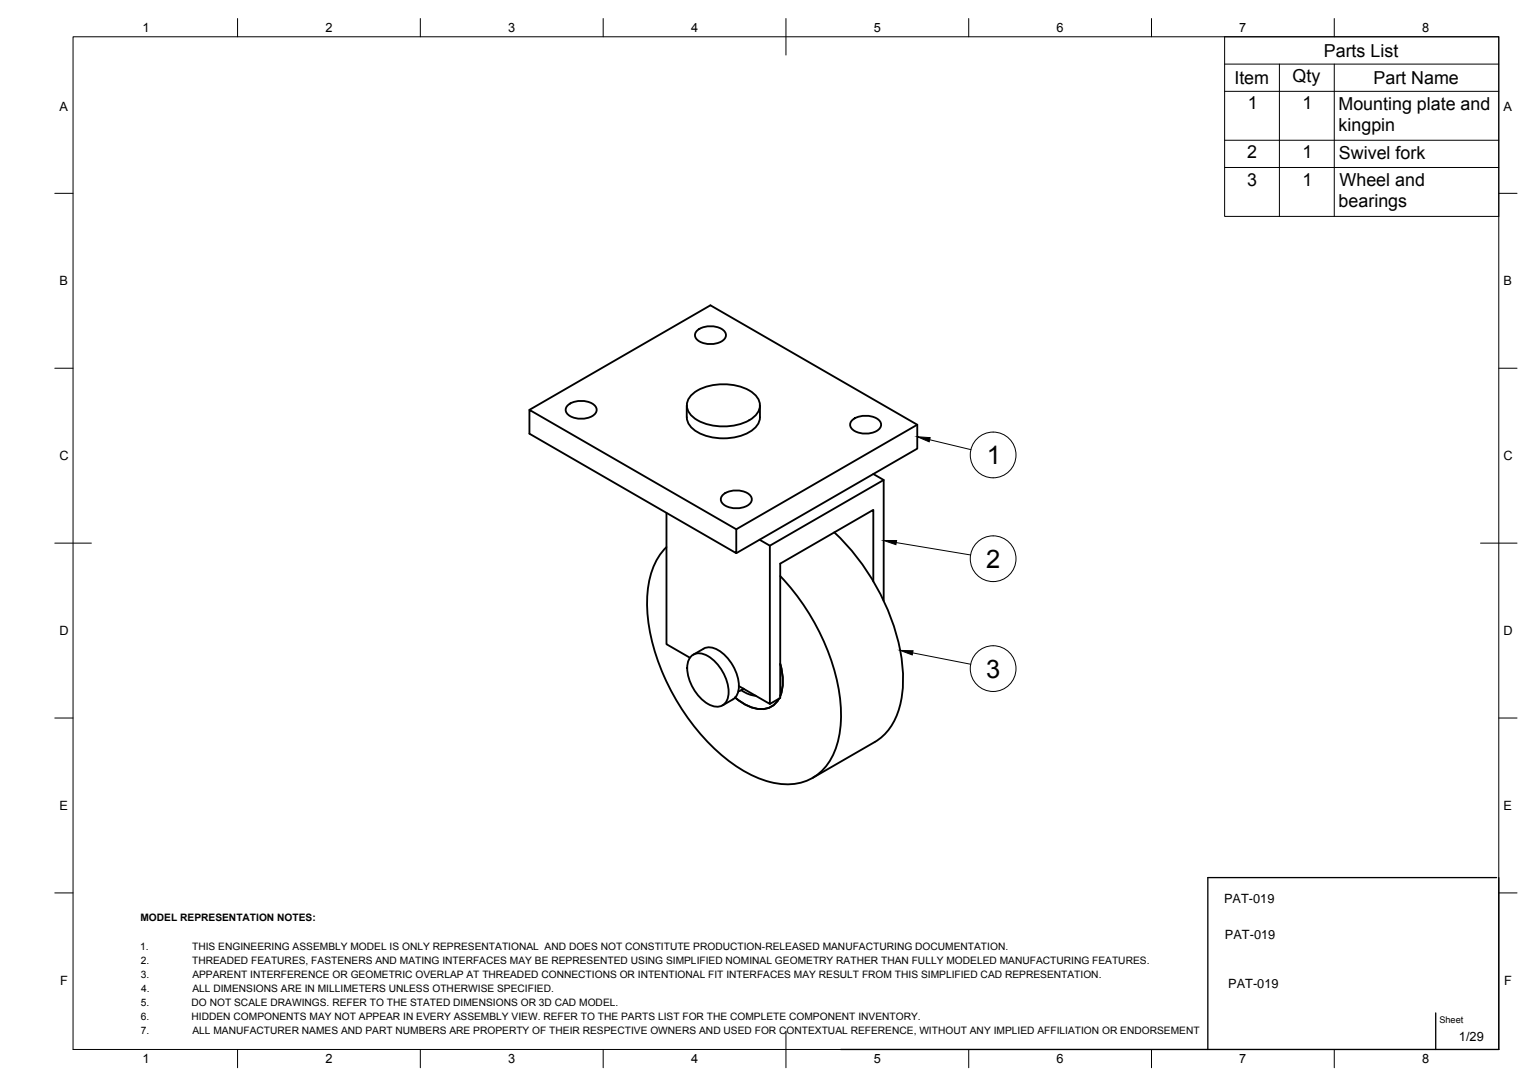
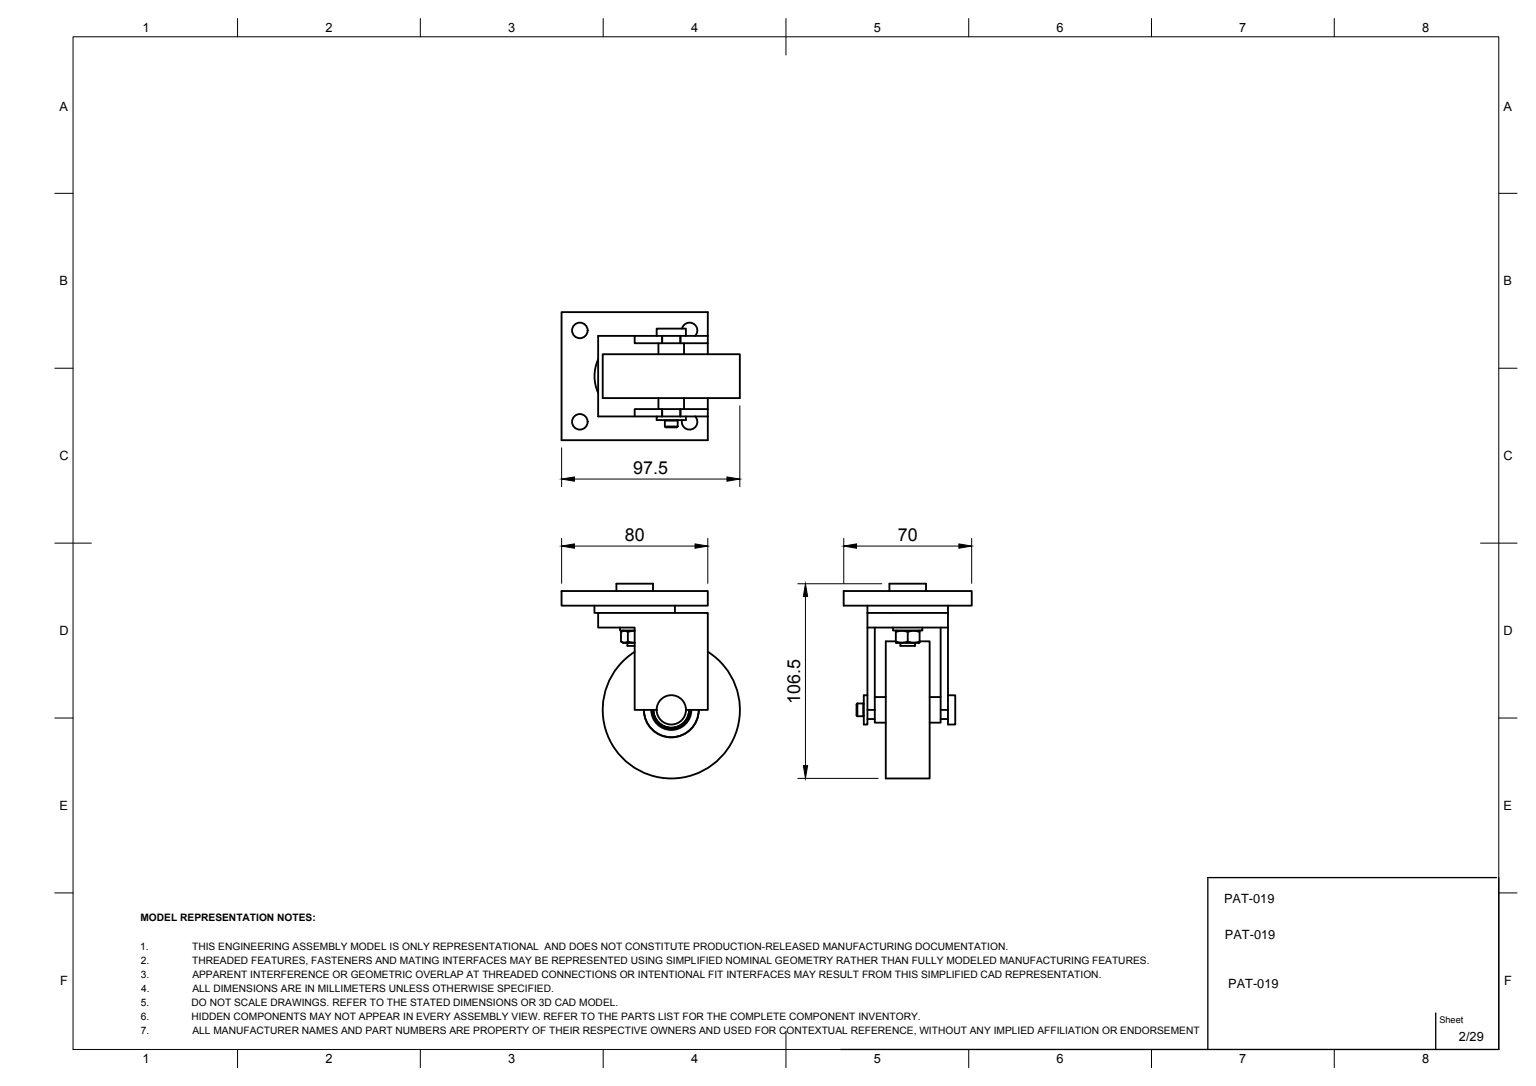
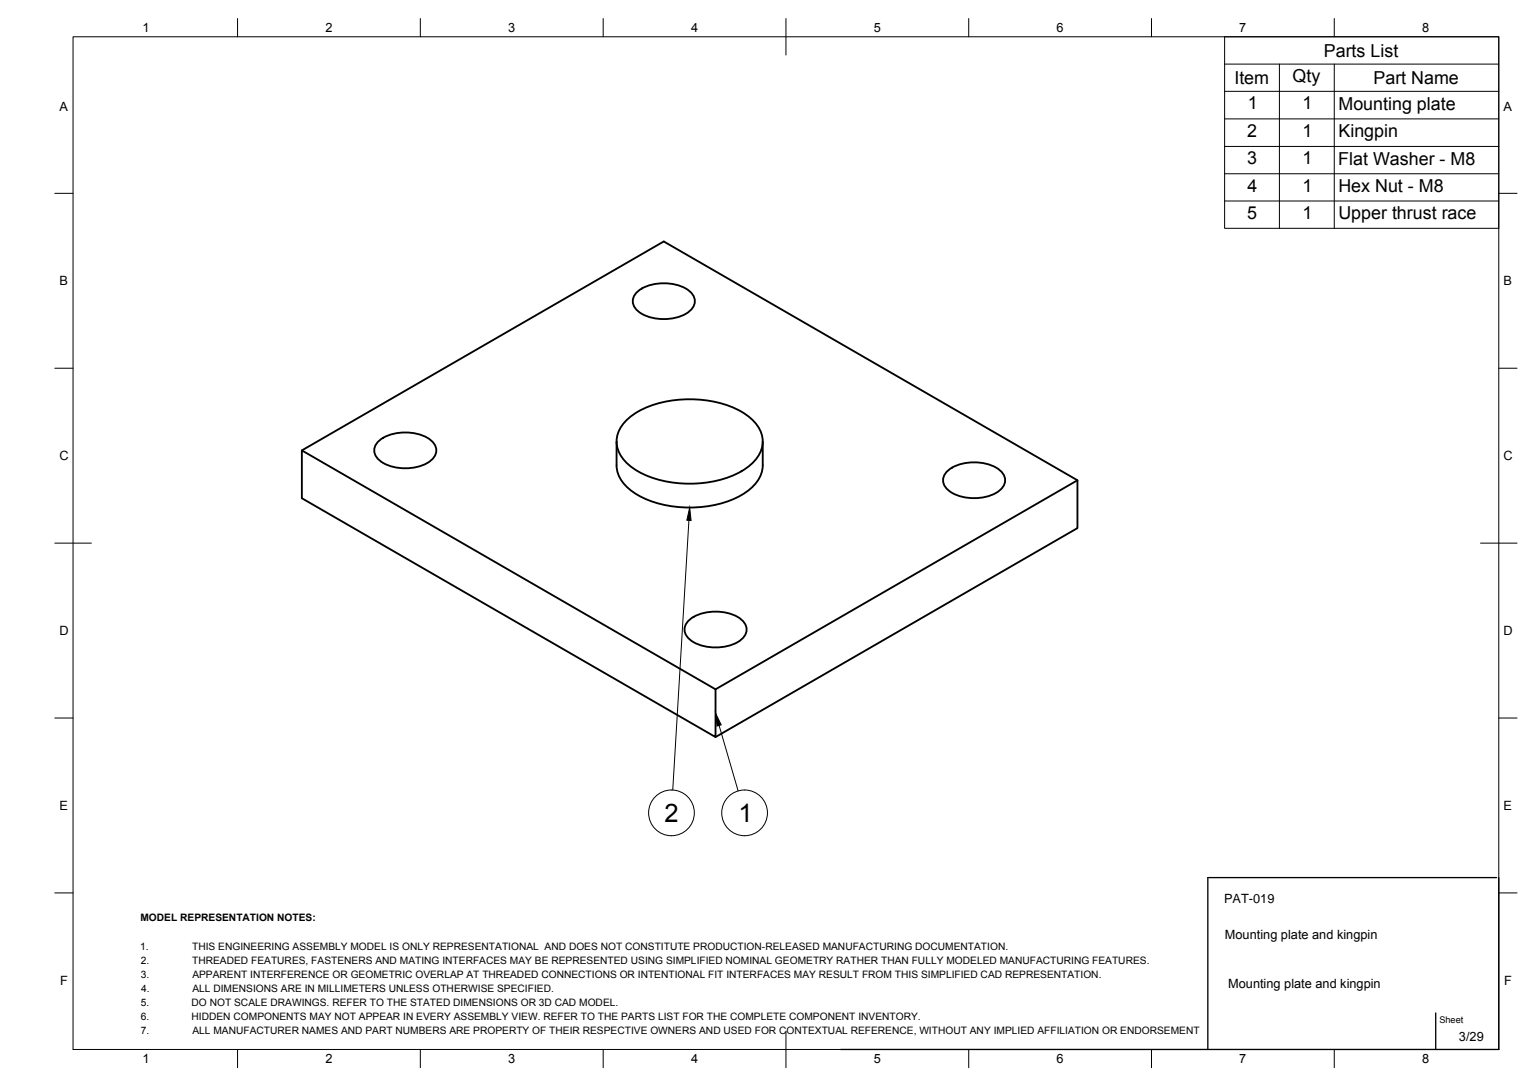
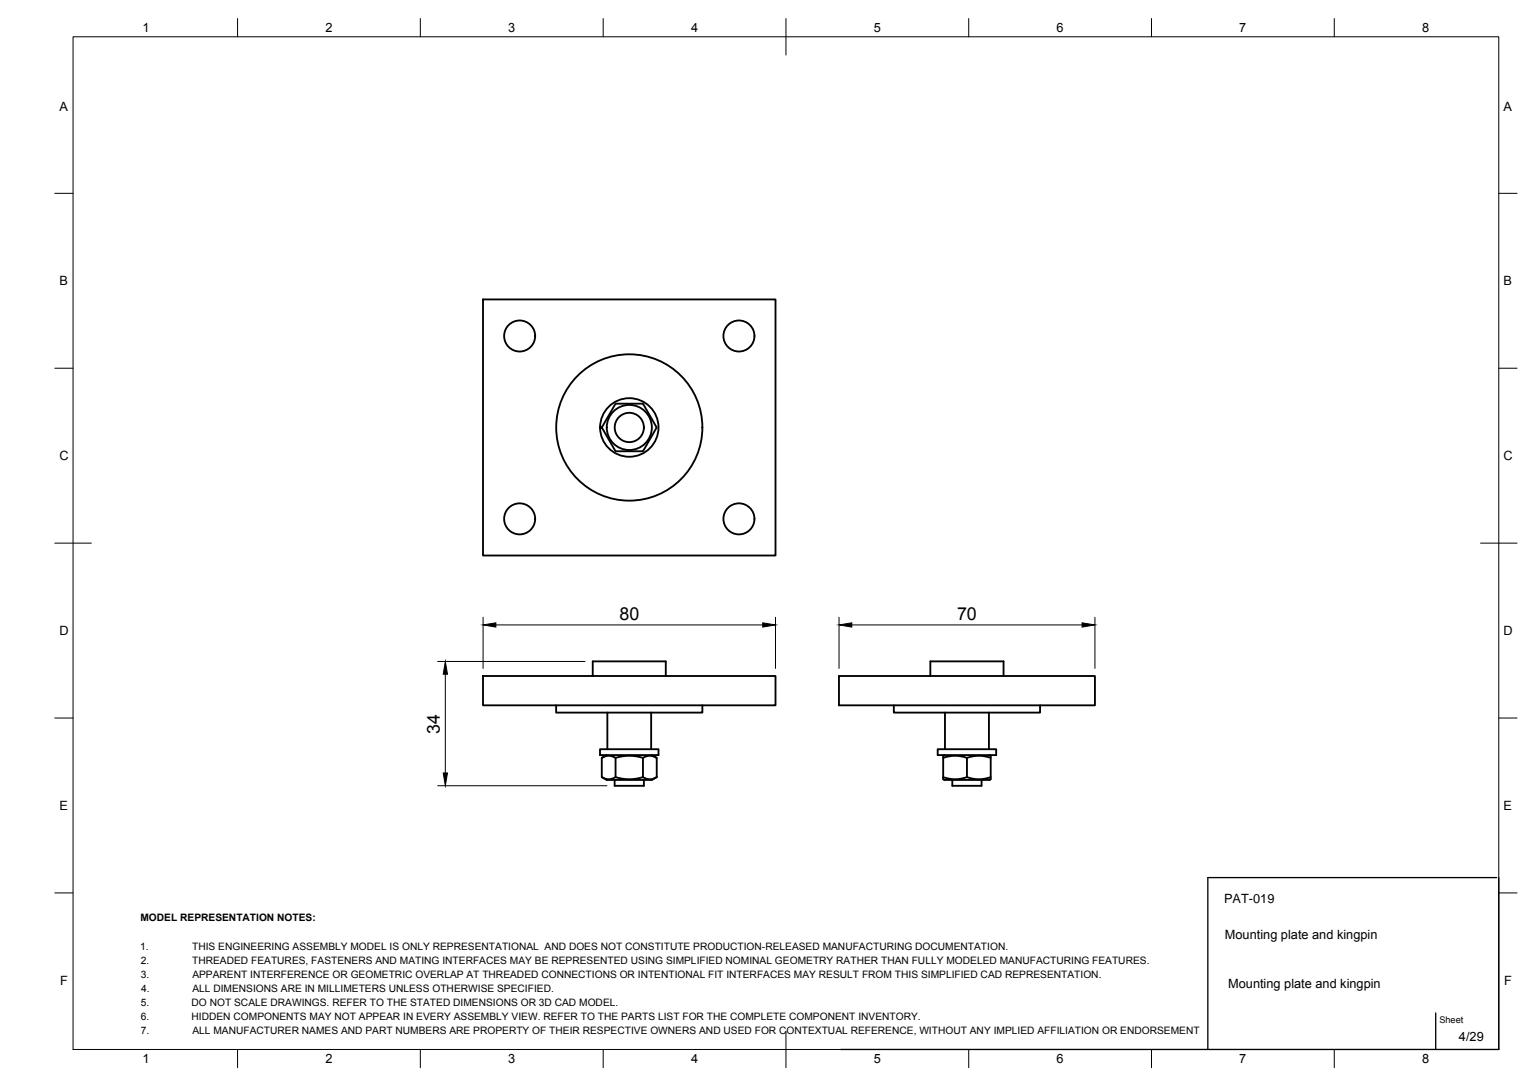
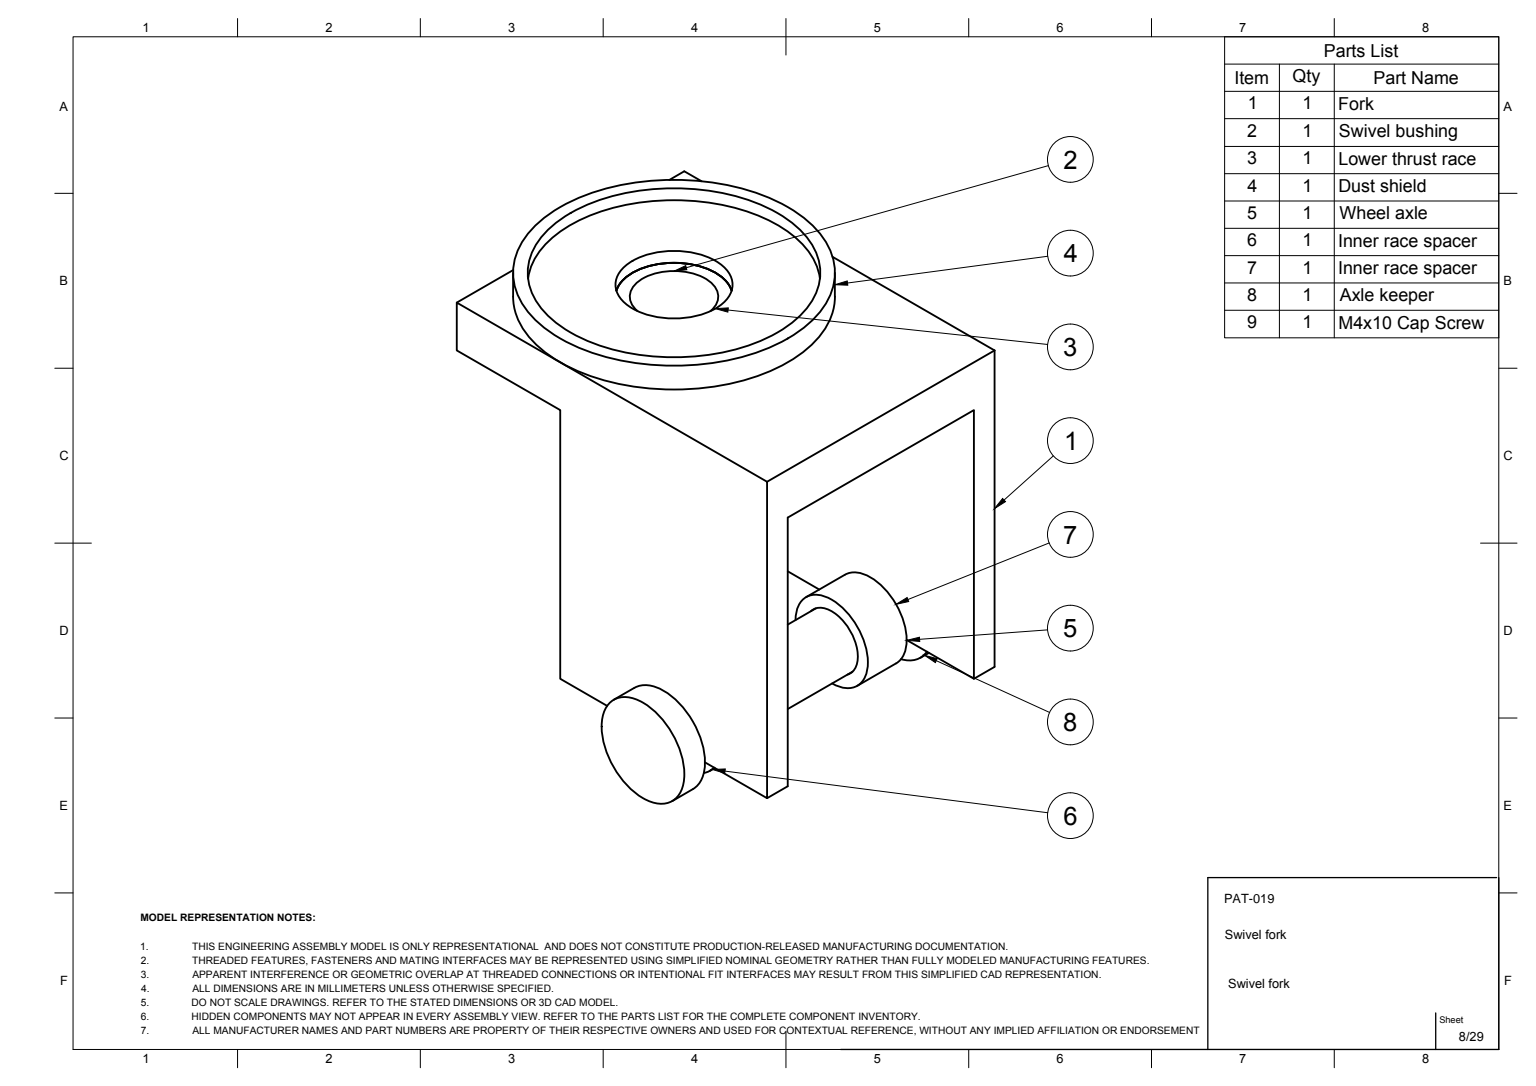
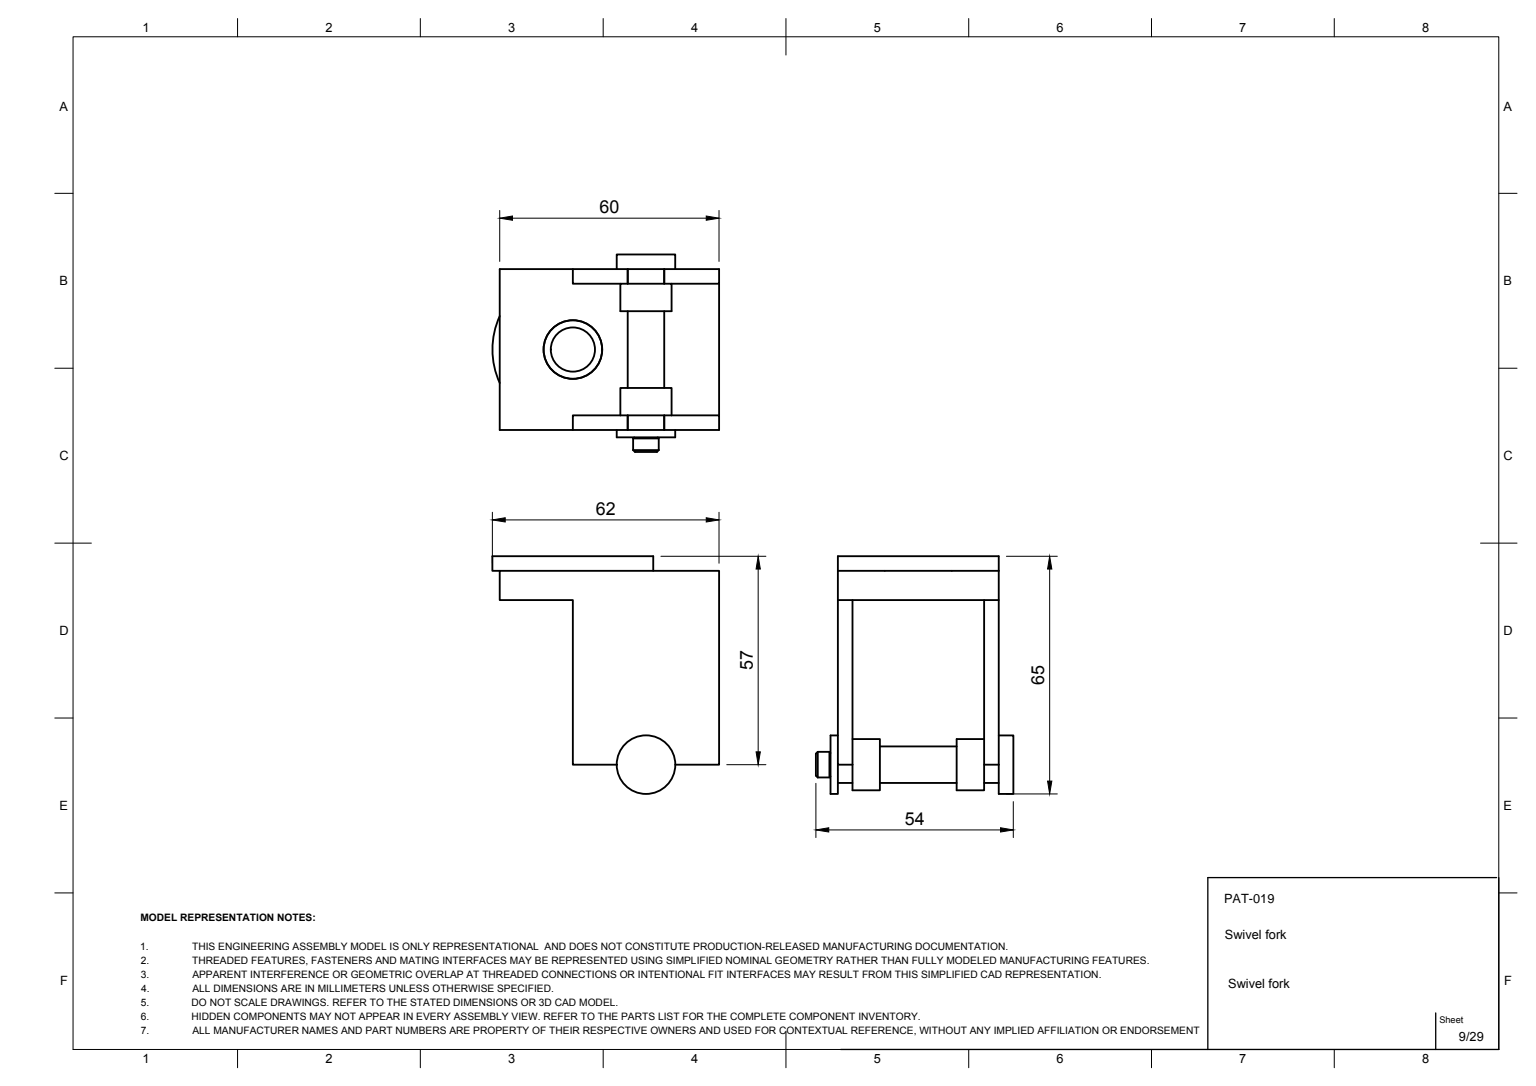
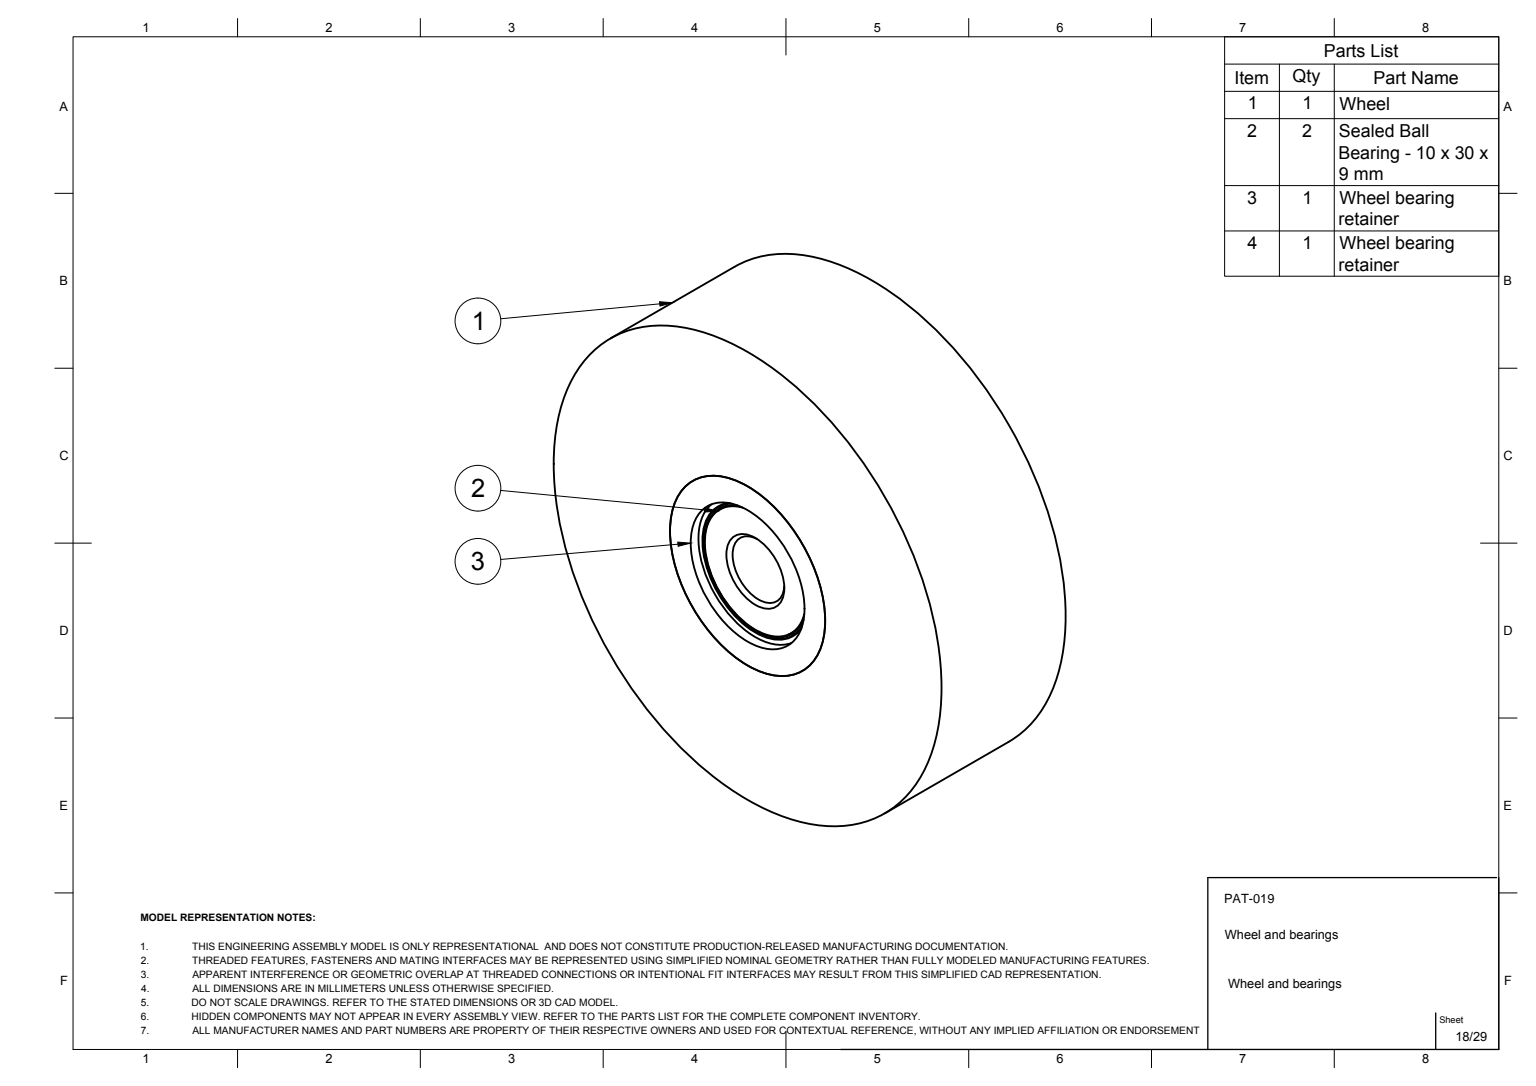
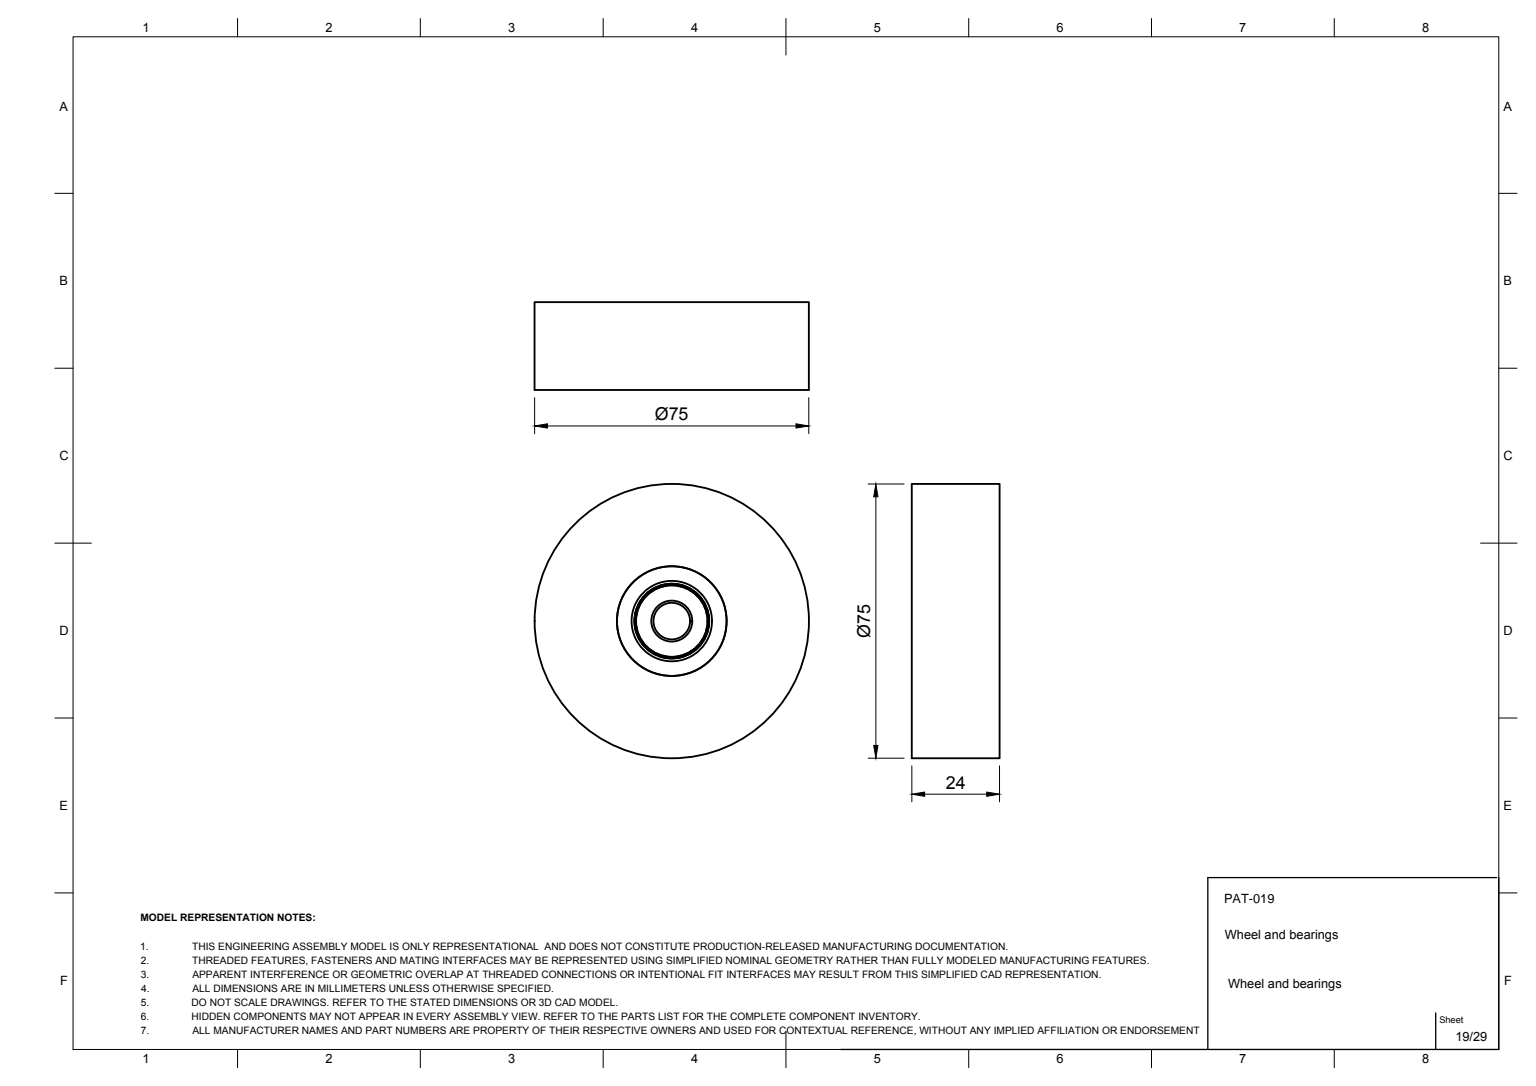
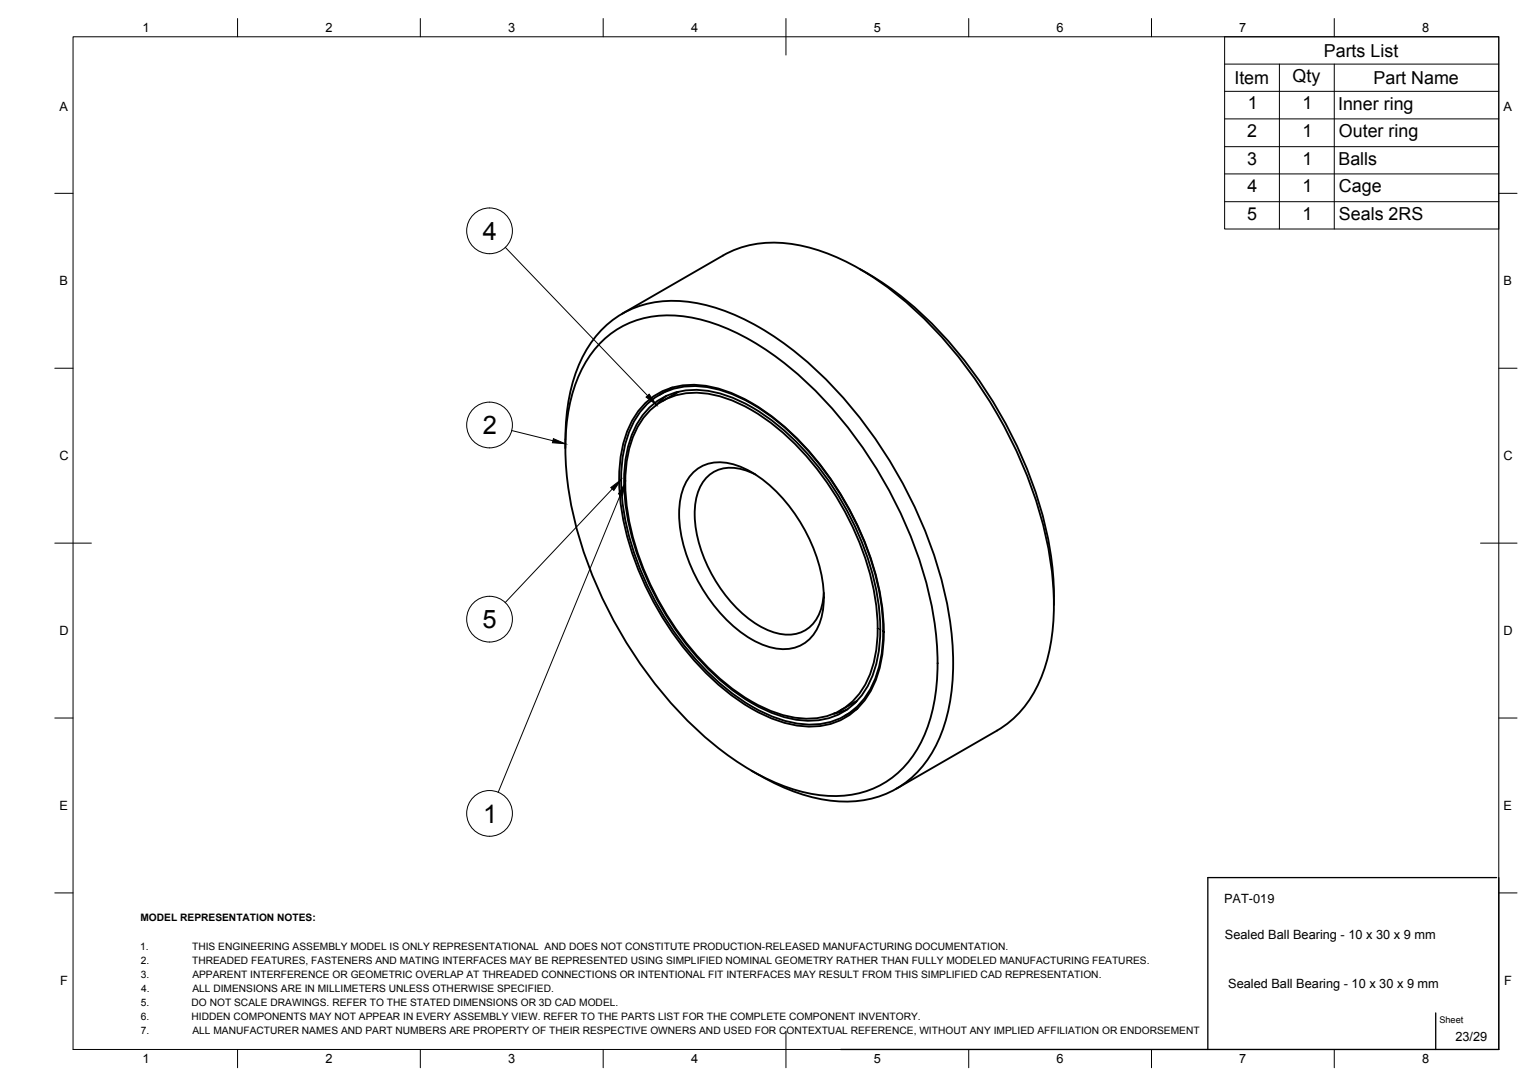
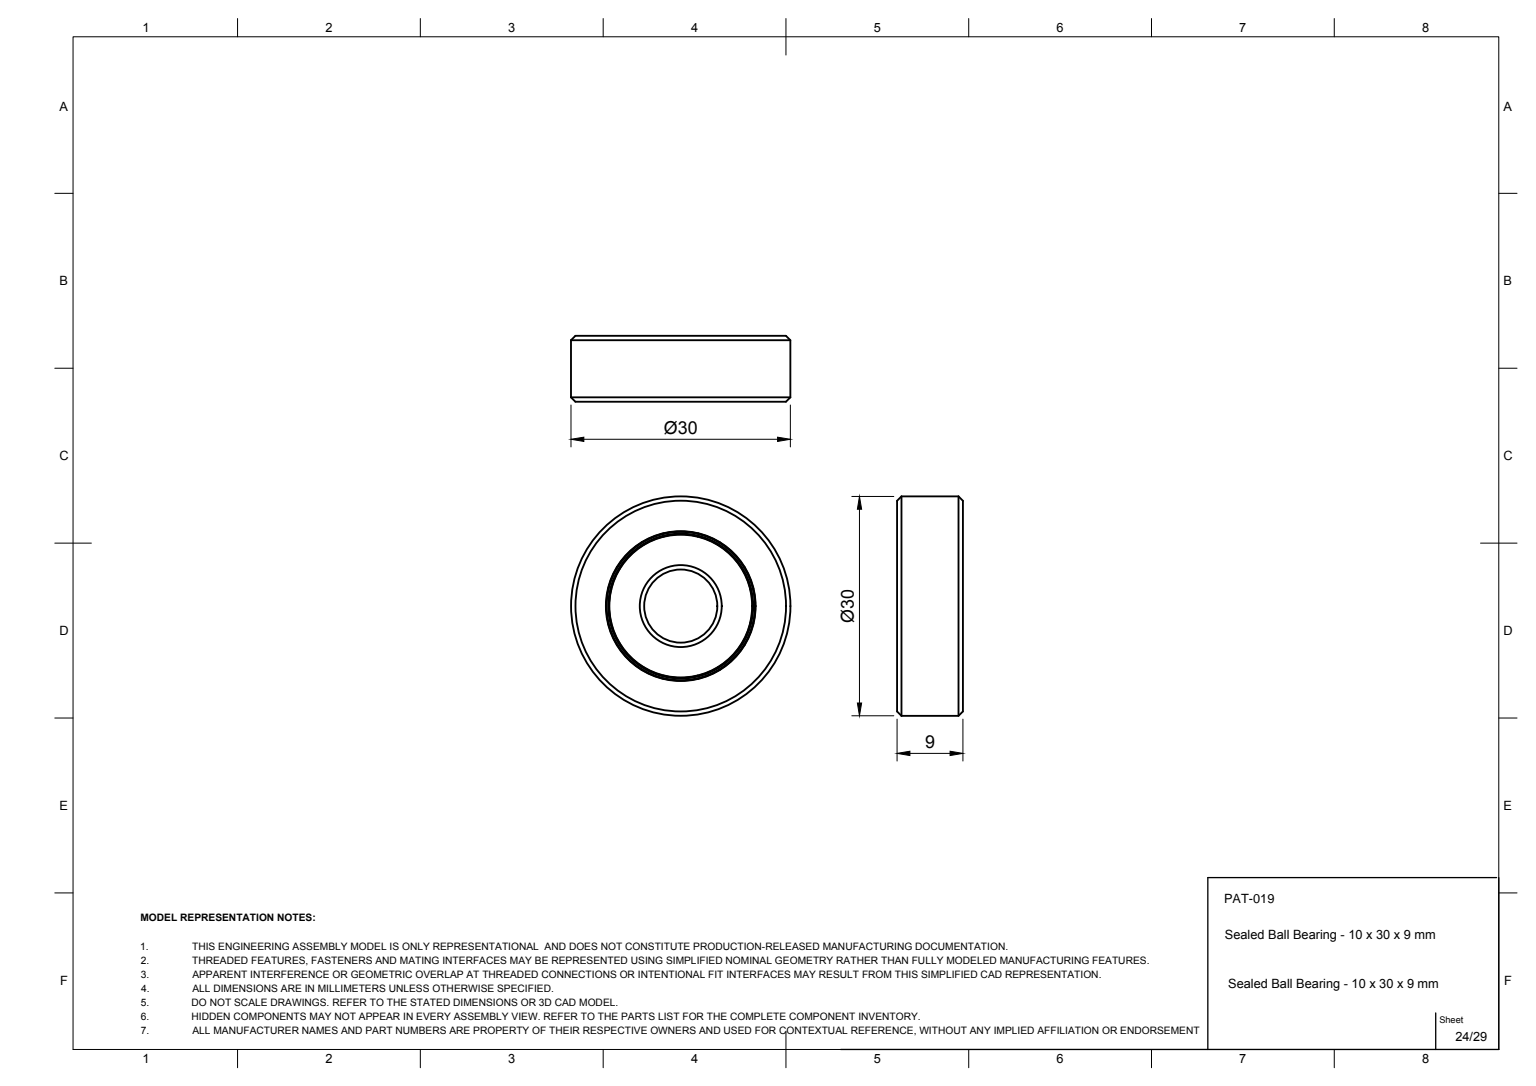
ISO-10303-21;
HEADER;
/* Generated by software containing ST-Developer
 * from STEP Tools, Inc. (www.steptools.com) 
 */

FILE_DESCRIPTION(
/* description */ ('Caster wheel assembly'),
/* implementation_level */ '2;1');

FILE_NAME(
/* name */ 'PAT-019',
/* time_stamp */ '2026-10-28T03:23:56-07:00',
/* author */ (''),
/* organization */ (''),
/* preprocessor_version */ 'ST-DEVELOPER v20.2',
/* originating_system */ 'Autodesk Translation Framework v15.17.0.0',
/* authorisation */ '');

FILE_SCHEMA (('AUTOMOTIVE_DESIGN { 1 0 10303 214 3 1 1 }'));
ENDSEC;

DATA;
#10=MECHANICAL_DESIGN_GEOMETRIC_PRESENTATION_REPRESENTATION('',(#222,#223,
#224,#225,#226,#227,#228,#229,#230,#231,#232,#233,#234,#235,#236,#237,#238,
#239,#240,#241,#242,#243,#244,#245,#246,#247,#248,#249,#250,#251),#5385);
#11=B_SPLINE_CURVE_WITH_KNOTS('',3,(#4844,#4845,#4846,#4847,#4848,#4849,
#4850,#4851,#4852,#4853,#4854,#4855,#4856,#4857,#4858,#4859,#4860,#4861,
#4862,#4863,#4864,#4865),.UNSPECIFIED.,.F.,.F.,(4,2,2,2,2,2,2,2,2,2,4),
(0.0473477652366656,0.126350602536658,0.189525903804987,0.252701205073317,
0.313298422430275,0.373895639787233,0.434492857144191,0.495090074501149,
0.558265375769478,0.621440677037807,0.7004435143378),.UNSPECIFIED.);
#12=B_SPLINE_CURVE_WITH_KNOTS('',3,(#4869,#4870,#4871,#4872,#4873,#4874,
#4875,#4876,#4877,#4878,#4879,#4880,#4881,#4882,#4883,#4884,#4885,#4886,
#4887,#4888,#4889,#4890),.UNSPECIFIED.,.F.,.F.,(4,2,2,2,2,2,2,2,2,2,4),
(0.0464897534940957,0.0852567806515119,0.170513561303024,0.246687263103517,
0.308657850341199,0.370628437578881,0.432599024816563,0.494569612054245,
0.570743313854739,0.656000094506251,0.694767121663666),.UNSPECIFIED.);
#13=B_SPLINE_CURVE_WITH_KNOTS('',3,(#4896,#4897,#4898,#4899,#4900,#4901,
#4902,#4903,#4904,#4905,#4906,#4907,#4908,#4909,#4910,#4911,#4912,#4913,
#4914,#4915,#4916,#4917),.UNSPECIFIED.,.F.,.F.,(4,2,2,2,2,2,2,2,2,2,4),
(0.0464897534940957,0.0852567806515118,0.170513561303024,0.246687263103517,
0.308657850341199,0.370628437578881,0.432599024816563,0.494569612054245,
0.570743313854738,0.65600009450625,0.694767121663666),.UNSPECIFIED.);
#14=B_SPLINE_CURVE_WITH_KNOTS('',3,(#4921,#4922,#4923,#4924,#4925,#4926,
#4927,#4928,#4929,#4930,#4931,#4932,#4933,#4934,#4935,#4936,#4937,#4938,
#4939,#4940,#4941,#4942),.UNSPECIFIED.,.F.,.F.,(4,2,2,2,2,2,2,2,2,2,4),
(0.0464897534940957,0.0852567806515119,0.170513561303024,0.246687263103517,
0.308657850341199,0.370628437578881,0.432599024816563,0.494569612054245,
0.570743313854739,0.656000094506251,0.694767121663666),.UNSPECIFIED.);
#15=B_SPLINE_CURVE_WITH_KNOTS('',3,(#4946,#4947,#4948,#4949,#4950,#4951,
#4952,#4953,#4954,#4955,#4956,#4957),.UNSPECIFIED.,.F.,.F.,(4,2,2,2,2,4),
(0.0464897534940957,0.0852567806515119,0.170513561303024,0.246687263103517,
0.308657850341199,0.370628437578881),.UNSPECIFIED.);
#16=B_SPLINE_CURVE_WITH_KNOTS('',3,(#4962,#4963,#4964,#4965,#4966,#4967,
#4968,#4969,#4970,#4971,#4972,#4973),.UNSPECIFIED.,.F.,.F.,(4,2,2,2,2,4),
(0.370628437578881,0.432599024816563,0.494569612054245,0.570743313854738,
0.65600009450625,0.694767121663666),.UNSPECIFIED.);
#17=B_SPLINE_CURVE_WITH_KNOTS('',3,(#4977,#4978,#4979,#4980,#4981,#4982,
#4983,#4984,#4985,#4986,#4987,#4988,#4989,#4990,#4991,#4992,#4993,#4994,
#4995,#4996,#4997,#4998),.UNSPECIFIED.,.F.,.F.,(4,2,2,2,2,2,2,2,2,2,4),
(0.0464897534940957,0.0852567806515121,0.170513561303024,0.246687263103518,
0.308657850341199,0.370628437578881,0.432599024816563,0.494569612054245,
0.570743313854738,0.65600009450625,0.694767121663666),.UNSPECIFIED.);
#18=B_SPLINE_CURVE_WITH_KNOTS('',3,(#5002,#5003,#5004,#5005,#5006,#5007,
#5008,#5009,#5010,#5011,#5012,#5013,#5014,#5015,#5016,#5017,#5018,#5019,
#5020,#5021,#5022,#5023),.UNSPECIFIED.,.F.,.F.,(4,2,2,2,2,2,2,2,2,2,4),
(0.0464897534940957,0.0852567806515119,0.170513561303024,0.246687263103517,
0.308657850341199,0.370628437578881,0.432599024816563,0.494569612054245,
0.570743313854738,0.65600009450625,0.694767121663667),.UNSPECIFIED.);
#19=B_SPLINE_CURVE_WITH_KNOTS('',3,(#5027,#5028,#5029,#5030,#5031,#5032,
#5033,#5034,#5035,#5036,#5037,#5038,#5039,#5040,#5041,#5042,#5043,#5044,
#5045,#5046,#5047,#5048),.UNSPECIFIED.,.F.,.F.,(4,2,2,2,2,2,2,2,2,2,4),
(0.0464897534940957,0.0852567806515119,0.170513561303024,0.246687263103517,
0.308657850341199,0.370628437578881,0.432599024816563,0.494569612054245,
0.570743313854738,0.65600009450625,0.694767121663666),.UNSPECIFIED.);
#20=B_SPLINE_CURVE_WITH_KNOTS('',3,(#5052,#5053,#5054,#5055,#5056,#5057,
#5058,#5059,#5060,#5061,#5062,#5063,#5064,#5065,#5066,#5067,#5068,#5069,
#5070,#5071,#5072,#5073),.UNSPECIFIED.,.F.,.F.,(4,2,2,2,2,2,2,2,2,2,4),
(0.0464897534940957,0.0852567806515119,0.170513561303024,0.246687263103517,
0.308657850341199,0.370628437578881,0.432599024816563,0.494569612054245,
0.570743313854739,0.656000094506251,0.694767121663667),.UNSPECIFIED.);
#21=B_SPLINE_CURVE_WITH_KNOTS('',3,(#5081,#5082,#5083,#5084,#5085,#5086,
#5087,#5088,#5089,#5090,#5091,#5092,#5093,#5094,#5095,#5096,#5097,#5098,
#5099,#5100,#5101,#5102),.UNSPECIFIED.,.F.,.F.,(4,2,2,2,2,2,2,2,2,2,4),
(0.0473477652366656,0.126350602536658,0.189525903804987,0.252701205073316,
0.313298422430274,0.373895639787232,0.434492857144191,0.495090074501149,
0.558265375769478,0.621440677037807,0.7004435143378),.UNSPECIFIED.);
#22=B_SPLINE_CURVE_WITH_KNOTS('',3,(#5110,#5111,#5112,#5113,#5114,#5115,
#5116,#5117,#5118,#5119,#5120,#5121,#5122,#5123,#5124,#5125,#5126,#5127,
#5128,#5129,#5130,#5131),.UNSPECIFIED.,.F.,.F.,(4,2,2,2,2,2,2,2,2,2,4),
(0.0473477652366656,0.126350602536658,0.189525903804987,0.252701205073317,
0.313298422430275,0.373895639787233,0.434492857144191,0.495090074501149,
0.558265375769478,0.621440677037807,0.7004435143378),.UNSPECIFIED.);
#23=B_SPLINE_CURVE_WITH_KNOTS('',3,(#5140,#5141,#5142,#5143,#5144,#5145,
#5146,#5147,#5148,#5149,#5150,#5151),.UNSPECIFIED.,.F.,.F.,(4,2,2,2,2,4),
(0.0473477652366656,0.126350602536658,0.189525903804987,0.252701205073316,
0.313298422430275,0.373895639787233),.UNSPECIFIED.);
#24=B_SPLINE_CURVE_WITH_KNOTS('',3,(#5153,#5154,#5155,#5156,#5157,#5158,
#5159,#5160,#5161,#5162,#5163,#5164),.UNSPECIFIED.,.F.,.F.,(4,2,2,2,2,4),
(0.373895639787233,0.434492857144191,0.495090074501149,0.558265375769478,
0.621440677037807,0.7004435143378),.UNSPECIFIED.);
#25=B_SPLINE_CURVE_WITH_KNOTS('',3,(#5171,#5172,#5173,#5174,#5175,#5176,
#5177,#5178,#5179,#5180,#5181,#5182,#5183,#5184,#5185,#5186,#5187,#5188,
#5189,#5190,#5191,#5192),.UNSPECIFIED.,.F.,.F.,(4,2,2,2,2,2,2,2,2,2,4),
(0.0473477652366656,0.126350602536658,0.189525903804987,0.252701205073316,
0.313298422430275,0.373895639787233,0.434492857144191,0.495090074501149,
0.558265375769478,0.621440677037807,0.7004435143378),.UNSPECIFIED.);
#26=B_SPLINE_CURVE_WITH_KNOTS('',3,(#5200,#5201,#5202,#5203,#5204,#5205,
#5206,#5207,#5208,#5209,#5210,#5211,#5212,#5213,#5214,#5215,#5216,#5217,
#5218,#5219,#5220,#5221),.UNSPECIFIED.,.F.,.F.,(4,2,2,2,2,2,2,2,2,2,4),
(0.0473477652366656,0.126350602536658,0.189525903804987,0.252701205073317,
0.313298422430275,0.373895639787233,0.434492857144191,0.495090074501149,
0.558265375769478,0.621440677037807,0.7004435143378),.UNSPECIFIED.);
#27=B_SPLINE_CURVE_WITH_KNOTS('',3,(#5229,#5230,#5231,#5232,#5233,#5234,
#5235,#5236,#5237,#5238,#5239,#5240,#5241,#5242,#5243,#5244,#5245,#5246,
#5247,#5248,#5249,#5250),.UNSPECIFIED.,.F.,.F.,(4,2,2,2,2,2,2,2,2,2,4),
(0.0473477652366656,0.126350602536658,0.189525903804987,0.252701205073316,
0.313298422430275,0.373895639787233,0.434492857144191,0.495090074501149,
0.558265375769478,0.621440677037807,0.7004435143378),.UNSPECIFIED.);
#28=B_SPLINE_CURVE_WITH_KNOTS('',3,(#5259,#5260,#5261,#5262,#5263,#5264,
#5265,#5266,#5267,#5268,#5269,#5270,#5271,#5272,#5273,#5274,#5275,#5276,
#5277,#5278,#5279,#5280),.UNSPECIFIED.,.F.,.F.,(4,2,2,2,2,2,2,2,2,2,4),
(0.0473477652366656,0.126350602536658,0.189525903804987,0.252701205073317,
0.313298422430275,0.373895639787233,0.434492857144191,0.495090074501149,
0.558265375769478,0.621440677037807,0.7004435143378),.UNSPECIFIED.);
#29=SPHERICAL_SURFACE('',#3204,0.23815);
#30=SPHERICAL_SURFACE('',#3206,0.23815);
#31=SPHERICAL_SURFACE('',#3208,0.23815);
#32=SPHERICAL_SURFACE('',#3210,0.23815);
#33=SPHERICAL_SURFACE('',#3212,0.23815);
#34=SPHERICAL_SURFACE('',#3214,0.23815);
#35=SPHERICAL_SURFACE('',#3216,0.23815);
#36=SPHERICAL_SURFACE('',#3218,0.23815);
#37=SPHERICAL_SURFACE('',#3221,0.247676);
#38=SPHERICAL_SURFACE('',#3237,0.247676);
#39=SPHERICAL_SURFACE('',#3242,0.247676);
#40=SPHERICAL_SURFACE('',#3247,0.247676);
#41=SPHERICAL_SURFACE('',#3252,0.247676);
#42=SPHERICAL_SURFACE('',#3257,0.247676);
#43=SPHERICAL_SURFACE('',#3262,0.247676);
#44=SPHERICAL_SURFACE('',#3270,0.247676);
#45=TOROIDAL_SURFACE('',#3164,1.,0.247676);
#46=TOROIDAL_SURFACE('',#3184,1.,0.247676);
#47=ORIENTED_CLOSED_SHELL('',*,#2662,.F.);
#48=BREP_WITH_VOIDS('Body1',#2663,(#47));
#49=ITEM_DEFINED_TRANSFORMATION($,$,#2925,#2995);
#50=ITEM_DEFINED_TRANSFORMATION($,$,#2947,#2996);
#51=ITEM_DEFINED_TRANSFORMATION($,$,#2961,#2997);
#52=ITEM_DEFINED_TRANSFORMATION($,$,#2970,#2998);
#53=ITEM_DEFINED_TRANSFORMATION($,$,#2979,#2999);
#54=ITEM_DEFINED_TRANSFORMATION($,$,#3001,#3117);
#55=ITEM_DEFINED_TRANSFORMATION($,$,#3025,#3118);
#56=ITEM_DEFINED_TRANSFORMATION($,$,#3034,#3119);
#57=ITEM_DEFINED_TRANSFORMATION($,$,#3043,#3120);
#58=ITEM_DEFINED_TRANSFORMATION($,$,#3052,#3121);
#59=ITEM_DEFINED_TRANSFORMATION($,$,#3066,#3122);
#60=ITEM_DEFINED_TRANSFORMATION($,$,#3075,#3123);
#61=ITEM_DEFINED_TRANSFORMATION($,$,#3084,#3124);
#62=ITEM_DEFINED_TRANSFORMATION($,$,#3093,#3125);
#63=ITEM_DEFINED_TRANSFORMATION($,$,#3163,#3291);
#64=ITEM_DEFINED_TRANSFORMATION($,$,#3183,#3292);
#65=ITEM_DEFINED_TRANSFORMATION($,$,#3203,#3293);
#66=ITEM_DEFINED_TRANSFORMATION($,$,#3220,#3294);
#67=ITEM_DEFINED_TRANSFORMATION($,$,#3274,#3295);
#68=ITEM_DEFINED_TRANSFORMATION($,$,#3127,#3296);
#69=ITEM_DEFINED_TRANSFORMATION($,$,#3144,#3297);
#70=ITEM_DEFINED_TRANSFORMATION($,$,#3153,#3298);
#71=ITEM_DEFINED_TRANSFORMATION($,$,#3162,#3299);
#72=ITEM_DEFINED_TRANSFORMATION($,$,#3162,#3300);
#73=ITEM_DEFINED_TRANSFORMATION($,$,#2924,#3301);
#74=ITEM_DEFINED_TRANSFORMATION($,$,#3000,#3302);
#75=ITEM_DEFINED_TRANSFORMATION($,$,#3126,#3303);
#76=(
REPRESENTATION_RELATIONSHIP($,$,#5473,#5472)
REPRESENTATION_RELATIONSHIP_WITH_TRANSFORMATION(#49)
SHAPE_REPRESENTATION_RELATIONSHIP()
);
#77=(
REPRESENTATION_RELATIONSHIP($,$,#5474,#5472)
REPRESENTATION_RELATIONSHIP_WITH_TRANSFORMATION(#50)
SHAPE_REPRESENTATION_RELATIONSHIP()
);
#78=(
REPRESENTATION_RELATIONSHIP($,$,#5475,#5472)
REPRESENTATION_RELATIONSHIP_WITH_TRANSFORMATION(#51)
SHAPE_REPRESENTATION_RELATIONSHIP()
);
#79=(
REPRESENTATION_RELATIONSHIP($,$,#5476,#5472)
REPRESENTATION_RELATIONSHIP_WITH_TRANSFORMATION(#52)
SHAPE_REPRESENTATION_RELATIONSHIP()
);
#80=(
REPRESENTATION_RELATIONSHIP($,$,#5477,#5472)
REPRESENTATION_RELATIONSHIP_WITH_TRANSFORMATION(#53)
SHAPE_REPRESENTATION_RELATIONSHIP()
);
#81=(
REPRESENTATION_RELATIONSHIP($,$,#5479,#5478)
REPRESENTATION_RELATIONSHIP_WITH_TRANSFORMATION(#54)
SHAPE_REPRESENTATION_RELATIONSHIP()
);
#82=(
REPRESENTATION_RELATIONSHIP($,$,#5480,#5478)
REPRESENTATION_RELATIONSHIP_WITH_TRANSFORMATION(#55)
SHAPE_REPRESENTATION_RELATIONSHIP()
);
#83=(
REPRESENTATION_RELATIONSHIP($,$,#5481,#5478)
REPRESENTATION_RELATIONSHIP_WITH_TRANSFORMATION(#56)
SHAPE_REPRESENTATION_RELATIONSHIP()
);
#84=(
REPRESENTATION_RELATIONSHIP($,$,#5482,#5478)
REPRESENTATION_RELATIONSHIP_WITH_TRANSFORMATION(#57)
SHAPE_REPRESENTATION_RELATIONSHIP()
);
#85=(
REPRESENTATION_RELATIONSHIP($,$,#5483,#5478)
REPRESENTATION_RELATIONSHIP_WITH_TRANSFORMATION(#58)
SHAPE_REPRESENTATION_RELATIONSHIP()
);
#86=(
REPRESENTATION_RELATIONSHIP($,$,#5484,#5478)
REPRESENTATION_RELATIONSHIP_WITH_TRANSFORMATION(#59)
SHAPE_REPRESENTATION_RELATIONSHIP()
);
#87=(
REPRESENTATION_RELATIONSHIP($,$,#5485,#5478)
REPRESENTATION_RELATIONSHIP_WITH_TRANSFORMATION(#60)
SHAPE_REPRESENTATION_RELATIONSHIP()
);
#88=(
REPRESENTATION_RELATIONSHIP($,$,#5486,#5478)
REPRESENTATION_RELATIONSHIP_WITH_TRANSFORMATION(#61)
SHAPE_REPRESENTATION_RELATIONSHIP()
);
#89=(
REPRESENTATION_RELATIONSHIP($,$,#5487,#5478)
REPRESENTATION_RELATIONSHIP_WITH_TRANSFORMATION(#62)
SHAPE_REPRESENTATION_RELATIONSHIP()
);
#90=(
REPRESENTATION_RELATIONSHIP($,$,#5493,#5492)
REPRESENTATION_RELATIONSHIP_WITH_TRANSFORMATION(#63)
SHAPE_REPRESENTATION_RELATIONSHIP()
);
#91=(
REPRESENTATION_RELATIONSHIP($,$,#5494,#5492)
REPRESENTATION_RELATIONSHIP_WITH_TRANSFORMATION(#64)
SHAPE_REPRESENTATION_RELATIONSHIP()
);
#92=(
REPRESENTATION_RELATIONSHIP($,$,#5495,#5492)
REPRESENTATION_RELATIONSHIP_WITH_TRANSFORMATION(#65)
SHAPE_REPRESENTATION_RELATIONSHIP()
);
#93=(
REPRESENTATION_RELATIONSHIP($,$,#5496,#5492)
REPRESENTATION_RELATIONSHIP_WITH_TRANSFORMATION(#66)
SHAPE_REPRESENTATION_RELATIONSHIP()
);
#94=(
REPRESENTATION_RELATIONSHIP($,$,#5497,#5492)
REPRESENTATION_RELATIONSHIP_WITH_TRANSFORMATION(#67)
SHAPE_REPRESENTATION_RELATIONSHIP()
);
#95=(
REPRESENTATION_RELATIONSHIP($,$,#5489,#5488)
REPRESENTATION_RELATIONSHIP_WITH_TRANSFORMATION(#68)
SHAPE_REPRESENTATION_RELATIONSHIP()
);
#96=(
REPRESENTATION_RELATIONSHIP($,$,#5490,#5488)
REPRESENTATION_RELATIONSHIP_WITH_TRANSFORMATION(#69)
SHAPE_REPRESENTATION_RELATIONSHIP()
);
#97=(
REPRESENTATION_RELATIONSHIP($,$,#5491,#5488)
REPRESENTATION_RELATIONSHIP_WITH_TRANSFORMATION(#70)
SHAPE_REPRESENTATION_RELATIONSHIP()
);
#98=(
REPRESENTATION_RELATIONSHIP($,$,#5492,#5488)
REPRESENTATION_RELATIONSHIP_WITH_TRANSFORMATION(#71)
SHAPE_REPRESENTATION_RELATIONSHIP()
);
#99=(
REPRESENTATION_RELATIONSHIP($,$,#5492,#5488)
REPRESENTATION_RELATIONSHIP_WITH_TRANSFORMATION(#72)
SHAPE_REPRESENTATION_RELATIONSHIP()
);
#100=(
REPRESENTATION_RELATIONSHIP($,$,#5472,#5471)
REPRESENTATION_RELATIONSHIP_WITH_TRANSFORMATION(#73)
SHAPE_REPRESENTATION_RELATIONSHIP()
);
#101=(
REPRESENTATION_RELATIONSHIP($,$,#5478,#5471)
REPRESENTATION_RELATIONSHIP_WITH_TRANSFORMATION(#74)
SHAPE_REPRESENTATION_RELATIONSHIP()
);
#102=(
REPRESENTATION_RELATIONSHIP($,$,#5488,#5471)
REPRESENTATION_RELATIONSHIP_WITH_TRANSFORMATION(#75)
SHAPE_REPRESENTATION_RELATIONSHIP()
);
#103=CONTEXT_DEPENDENT_SHAPE_REPRESENTATION(#76,#5424);
#104=CONTEXT_DEPENDENT_SHAPE_REPRESENTATION(#77,#5425);
#105=CONTEXT_DEPENDENT_SHAPE_REPRESENTATION(#78,#5426);
#106=CONTEXT_DEPENDENT_SHAPE_REPRESENTATION(#79,#5427);
#107=CONTEXT_DEPENDENT_SHAPE_REPRESENTATION(#80,#5428);
#108=CONTEXT_DEPENDENT_SHAPE_REPRESENTATION(#81,#5439);
#109=CONTEXT_DEPENDENT_SHAPE_REPRESENTATION(#82,#5440);
#110=CONTEXT_DEPENDENT_SHAPE_REPRESENTATION(#83,#5441);
#111=CONTEXT_DEPENDENT_SHAPE_REPRESENTATION(#84,#5442);
#112=CONTEXT_DEPENDENT_SHAPE_REPRESENTATION(#85,#5443);
#113=CONTEXT_DEPENDENT_SHAPE_REPRESENTATION(#86,#5444);
#114=CONTEXT_DEPENDENT_SHAPE_REPRESENTATION(#87,#5445);
#115=CONTEXT_DEPENDENT_SHAPE_REPRESENTATION(#88,#5446);
#116=CONTEXT_DEPENDENT_SHAPE_REPRESENTATION(#89,#5447);
#117=CONTEXT_DEPENDENT_SHAPE_REPRESENTATION(#90,#5458);
#118=CONTEXT_DEPENDENT_SHAPE_REPRESENTATION(#91,#5459);
#119=CONTEXT_DEPENDENT_SHAPE_REPRESENTATION(#92,#5460);
#120=CONTEXT_DEPENDENT_SHAPE_REPRESENTATION(#93,#5461);
#121=CONTEXT_DEPENDENT_SHAPE_REPRESENTATION(#94,#5462);
#122=CONTEXT_DEPENDENT_SHAPE_REPRESENTATION(#95,#5463);
#123=CONTEXT_DEPENDENT_SHAPE_REPRESENTATION(#96,#5464);
#124=CONTEXT_DEPENDENT_SHAPE_REPRESENTATION(#97,#5465);
#125=CONTEXT_DEPENDENT_SHAPE_REPRESENTATION(#98,#5466);
#126=CONTEXT_DEPENDENT_SHAPE_REPRESENTATION(#99,#5467);
#127=CONTEXT_DEPENDENT_SHAPE_REPRESENTATION(#100,#5468);
#128=CONTEXT_DEPENDENT_SHAPE_REPRESENTATION(#101,#5469);
#129=CONTEXT_DEPENDENT_SHAPE_REPRESENTATION(#102,#5470);
#130=NEXT_ASSEMBLY_USAGE_OCCURRENCE('Mounting plate:1',
'Mounting plate:1','Mounting plate:1',#5500,#5501,'Mounting plate:1');
#131=NEXT_ASSEMBLY_USAGE_OCCURRENCE('Kingpin:1','Kingpin:1','Kingpin:1',
#5500,#5502,'Kingpin:1');
#132=NEXT_ASSEMBLY_USAGE_OCCURRENCE('Upper thrust race:1',
'Upper thrust race:1','Upper thrust race:1',#5500,#5503,
'Upper thrust race:1');
#133=NEXT_ASSEMBLY_USAGE_OCCURRENCE('Flat Washer - M8:2',
'Flat Washer - M8:2','Flat Washer - M8:2',#5500,#5504,
'Flat Washer - M8:2');
#134=NEXT_ASSEMBLY_USAGE_OCCURRENCE('Hex Nut - M8:2','Hex Nut - M8:2',
'Hex Nut - M8:2',#5500,#5505,'Hex Nut - M8:2');
#135=NEXT_ASSEMBLY_USAGE_OCCURRENCE('Fork:1','Fork:1','Fork:1',#5506,#5507,
'Fork:1');
#136=NEXT_ASSEMBLY_USAGE_OCCURRENCE('Swivel bushing:1',
'Swivel bushing:1','Swivel bushing:1',#5506,#5508,'Swivel bushing:1');
#137=NEXT_ASSEMBLY_USAGE_OCCURRENCE('Lower thrust race:1',
'Lower thrust race:1','Lower thrust race:1',#5506,#5509,
'Lower thrust race:1');
#138=NEXT_ASSEMBLY_USAGE_OCCURRENCE('Dust shield:1','Dust shield:1',
'Dust shield:1',#5506,#5510,'Dust shield:1');
#139=NEXT_ASSEMBLY_USAGE_OCCURRENCE('Wheel axle:1','Wheel axle:1',
'Wheel axle:1',#5506,#5511,'Wheel axle:1');
#140=NEXT_ASSEMBLY_USAGE_OCCURRENCE('Inner race spacer:1',
'Inner race spacer:1','Inner race spacer:1',#5506,#5512,
'Inner race spacer:1');
#141=NEXT_ASSEMBLY_USAGE_OCCURRENCE('Inner race spacer (1):1',
'Inner race spacer (1):1','Inner race spacer (1):1',#5506,#5513,
'Inner race spacer (1):1');
#142=NEXT_ASSEMBLY_USAGE_OCCURRENCE('Axle keeper:1','Axle keeper:1',
'Axle keeper:1',#5506,#5514,'Axle keeper:1');
#143=NEXT_ASSEMBLY_USAGE_OCCURRENCE('M4x10 Cap Screw:2',
'M4x10 Cap Screw:2','M4x10 Cap Screw:2',#5506,#5515,'M4x10 Cap Screw:2');
#144=NEXT_ASSEMBLY_USAGE_OCCURRENCE('Inner ring:1','Inner ring:1',
'Inner ring:1',#5520,#5521,'Inner ring:1');
#145=NEXT_ASSEMBLY_USAGE_OCCURRENCE('Outer ring:1','Outer ring:1',
'Outer ring:1',#5520,#5522,'Outer ring:1');
#146=NEXT_ASSEMBLY_USAGE_OCCURRENCE('Balls:1','Balls:1','Balls:1',#5520,
#5523,'Balls:1');
#147=NEXT_ASSEMBLY_USAGE_OCCURRENCE('Cage:1','Cage:1','Cage:1',#5520,#5524,
'Cage:1');
#148=NEXT_ASSEMBLY_USAGE_OCCURRENCE('Seals 2RS:1','Seals 2RS:1',
'Seals 2RS:1',#5520,#5525,'Seals 2RS:1');
#149=NEXT_ASSEMBLY_USAGE_OCCURRENCE('Wheel:1','Wheel:1','Wheel:1',#5516,
#5517,'Wheel:1');
#150=NEXT_ASSEMBLY_USAGE_OCCURRENCE('Wheel bearing retainer:1',
'Wheel bearing retainer:1','Wheel bearing retainer:1',#5516,#5518,
'Wheel bearing retainer:1');
#151=NEXT_ASSEMBLY_USAGE_OCCURRENCE('Wheel bearing retainer (1):1',
'Wheel bearing retainer (1):1','Wheel bearing retainer (1):1',#5516,#5519,
'Wheel bearing retainer (1):1');
#152=NEXT_ASSEMBLY_USAGE_OCCURRENCE(
'Sealed Ball Bearing - 10 x 30 x 9 mm:2',
'Sealed Ball Bearing - 10 x 30 x 9 mm:2',
'Sealed Ball Bearing - 10 x 30 x 9 mm:2',#5516,#5520,
'Sealed Ball Bearing - 10 x 30 x 9 mm:2');
#153=NEXT_ASSEMBLY_USAGE_OCCURRENCE(
'Sealed Ball Bearing - 10 x 30 x 9 mm:3',
'Sealed Ball Bearing - 10 x 30 x 9 mm:3',
'Sealed Ball Bearing - 10 x 30 x 9 mm:3',#5516,#5520,
'Sealed Ball Bearing - 10 x 30 x 9 mm:3');
#154=NEXT_ASSEMBLY_USAGE_OCCURRENCE('Mounting plate and kingpin:1',
'Mounting plate and kingpin:1','Mounting plate and kingpin:1',#5499,#5500,
'Mounting plate and kingpin:1');
#155=NEXT_ASSEMBLY_USAGE_OCCURRENCE('Swivel fork:1','Swivel fork:1',
'Swivel fork:1',#5499,#5506,'Swivel fork:1');
#156=NEXT_ASSEMBLY_USAGE_OCCURRENCE('Wheel and bearings:1',
'Wheel and bearings:1','Wheel and bearings:1',#5499,#5516,
'Wheel and bearings:1');
#157=(
BOUNDED_CURVE()
B_SPLINE_CURVE(2,(#4316,#4317,#4318),.UNSPECIFIED.,.F.,.F.)
B_SPLINE_CURVE_WITH_KNOTS((3,3),(0.14973948338295,0.97160236658079),
 .UNSPECIFIED.)
CURVE()
GEOMETRIC_REPRESENTATION_ITEM()
RATIONAL_B_SPLINE_CURVE((1.07140024848292,1.23714644374248,1.07140024848292))
REPRESENTATION_ITEM('')
);
#158=(
BOUNDED_CURVE()
B_SPLINE_CURVE(2,(#4320,#4321,#4322),.UNSPECIFIED.,.F.,.F.)
B_SPLINE_CURVE_WITH_KNOTS((3,3),(0.14973948338295,0.971602366580789),
 .UNSPECIFIED.)
CURVE()
GEOMETRIC_REPRESENTATION_ITEM()
RATIONAL_B_SPLINE_CURVE((1.07140024848292,1.23714644374248,1.07140024848292))
REPRESENTATION_ITEM('')
);
#159=(
BOUNDED_CURVE()
B_SPLINE_CURVE(2,(#4327,#4328,#4329),.UNSPECIFIED.,.F.,.F.)
B_SPLINE_CURVE_WITH_KNOTS((3,3),(0.14973948338295,0.97160236658079),
 .UNSPECIFIED.)
CURVE()
GEOMETRIC_REPRESENTATION_ITEM()
RATIONAL_B_SPLINE_CURVE((1.07140024848292,1.23714644374248,1.07140024848292))
REPRESENTATION_ITEM('')
);
#160=(
BOUNDED_CURVE()
B_SPLINE_CURVE(2,(#4331,#4332,#4333),.UNSPECIFIED.,.F.,.F.)
B_SPLINE_CURVE_WITH_KNOTS((3,3),(0.14973948338295,0.97160236658079),
 .UNSPECIFIED.)
CURVE()
GEOMETRIC_REPRESENTATION_ITEM()
RATIONAL_B_SPLINE_CURVE((1.07140024848292,1.23714644374248,1.07140024848292))
REPRESENTATION_ITEM('')
);
#161=(
BOUNDED_CURVE()
B_SPLINE_CURVE(2,(#4335,#4336,#4337),.UNSPECIFIED.,.F.,.F.)
B_SPLINE_CURVE_WITH_KNOTS((3,3),(0.14973948338295,0.971602366580789),
 .UNSPECIFIED.)
CURVE()
GEOMETRIC_REPRESENTATION_ITEM()
RATIONAL_B_SPLINE_CURVE((1.07140024848292,1.23714644374248,1.07140024848292))
REPRESENTATION_ITEM('')
);
#162=(
BOUNDED_CURVE()
B_SPLINE_CURVE(2,(#4338,#4339,#4340),.UNSPECIFIED.,.F.,.F.)
B_SPLINE_CURVE_WITH_KNOTS((3,3),(0.14973948338295,0.97160236658079),
 .UNSPECIFIED.)
CURVE()
GEOMETRIC_REPRESENTATION_ITEM()
RATIONAL_B_SPLINE_CURVE((1.07140024848292,1.23714644374248,1.07140024848292))
REPRESENTATION_ITEM('')
);
#163=(
BOUNDED_CURVE()
B_SPLINE_CURVE(2,(#4347,#4348,#4349),.UNSPECIFIED.,.F.,.F.)
B_SPLINE_CURVE_WITH_KNOTS((3,3),(0.14973948338295,0.97160236658079),
 .UNSPECIFIED.)
CURVE()
GEOMETRIC_REPRESENTATION_ITEM()
RATIONAL_B_SPLINE_CURVE((1.07140024848292,1.23714644374248,1.07140024848292))
REPRESENTATION_ITEM('')
);
#164=(
BOUNDED_CURVE()
B_SPLINE_CURVE(2,(#4351,#4352,#4353),.UNSPECIFIED.,.F.,.F.)
B_SPLINE_CURVE_WITH_KNOTS((3,3),(0.14973948338295,0.97160236658079),
 .UNSPECIFIED.)
CURVE()
GEOMETRIC_REPRESENTATION_ITEM()
RATIONAL_B_SPLINE_CURVE((1.07140024848292,1.23714644374248,1.07140024848292))
REPRESENTATION_ITEM('')
);
#165=(
BOUNDED_CURVE()
B_SPLINE_CURVE(2,(#4355,#4356,#4357),.UNSPECIFIED.,.F.,.F.)
B_SPLINE_CURVE_WITH_KNOTS((3,3),(0.14973948338295,0.971602366580789),
 .UNSPECIFIED.)
CURVE()
GEOMETRIC_REPRESENTATION_ITEM()
RATIONAL_B_SPLINE_CURVE((1.07140024848292,1.23714644374248,1.07140024848292))
REPRESENTATION_ITEM('')
);
#166=(
BOUNDED_CURVE()
B_SPLINE_CURVE(2,(#4359,#4360,#4361),.UNSPECIFIED.,.F.,.F.)
B_SPLINE_CURVE_WITH_KNOTS((3,3),(0.14973948338295,0.97160236658079),
 .UNSPECIFIED.)
CURVE()
GEOMETRIC_REPRESENTATION_ITEM()
RATIONAL_B_SPLINE_CURVE((1.07140024848292,1.23714644374248,1.07140024848292))
REPRESENTATION_ITEM('')
);
#167=(
BOUNDED_CURVE()
B_SPLINE_CURVE(2,(#4363,#4364,#4365),.UNSPECIFIED.,.F.,.F.)
B_SPLINE_CURVE_WITH_KNOTS((3,3),(0.14973948338295,0.97160236658079),
 .UNSPECIFIED.)
CURVE()
GEOMETRIC_REPRESENTATION_ITEM()
RATIONAL_B_SPLINE_CURVE((1.07140024848292,1.23714644374248,1.07140024848292))
REPRESENTATION_ITEM('')
);
#168=(
BOUNDED_CURVE()
B_SPLINE_CURVE(2,(#4366,#4367,#4368),.UNSPECIFIED.,.F.,.F.)
B_SPLINE_CURVE_WITH_KNOTS((3,3),(0.14973948338295,0.971602366580789),
 .UNSPECIFIED.)
CURVE()
GEOMETRIC_REPRESENTATION_ITEM()
RATIONAL_B_SPLINE_CURVE((1.07140024848292,1.23714644374248,1.07140024848292))
REPRESENTATION_ITEM('')
);
#169=CONICAL_SURFACE('',#2980,0.734027674973257,1.0471975511966);
#170=CONICAL_SURFACE('',#2982,0.734027674973257,1.0471975511966);
#171=CONICAL_SURFACE('',#3106,0.325,0.785398163397448);
#172=CONICAL_SURFACE('',#3110,0.335,0.785398163397448);
#173=CONICAL_SURFACE('',#3114,0.21,0.463647609000806);
#174=CONICAL_SURFACE('',#3175,0.53,0.785398163397448);
#175=CONICAL_SURFACE('',#3182,0.53,0.785398163397448);
#176=CONICAL_SURFACE('',#3195,1.47,0.785398163397449);
#177=CONICAL_SURFACE('',#3199,1.47,0.785398163397449);
#178=SHAPE_REPRESENTATION_RELATIONSHIP('SRR','None',#5473,#200);
#179=SHAPE_REPRESENTATION_RELATIONSHIP('SRR','None',#5474,#201);
#180=SHAPE_REPRESENTATION_RELATIONSHIP('SRR','None',#5475,#202);
#181=SHAPE_REPRESENTATION_RELATIONSHIP('SRR','None',#5476,#203);
#182=SHAPE_REPRESENTATION_RELATIONSHIP('SRR','None',#5477,#204);
#183=SHAPE_REPRESENTATION_RELATIONSHIP('SRR','None',#5479,#205);
#184=SHAPE_REPRESENTATION_RELATIONSHIP('SRR','None',#5480,#206);
#185=SHAPE_REPRESENTATION_RELATIONSHIP('SRR','None',#5481,#207);
#186=SHAPE_REPRESENTATION_RELATIONSHIP('SRR','None',#5482,#208);
#187=SHAPE_REPRESENTATION_RELATIONSHIP('SRR','None',#5483,#209);
#188=SHAPE_REPRESENTATION_RELATIONSHIP('SRR','None',#5484,#210);
#189=SHAPE_REPRESENTATION_RELATIONSHIP('SRR','None',#5485,#211);
#190=SHAPE_REPRESENTATION_RELATIONSHIP('SRR','None',#5486,#212);
#191=SHAPE_REPRESENTATION_RELATIONSHIP('SRR','None',#5487,#213);
#192=SHAPE_REPRESENTATION_RELATIONSHIP('SRR','None',#5489,#214);
#193=SHAPE_REPRESENTATION_RELATIONSHIP('SRR','None',#5490,#215);
#194=SHAPE_REPRESENTATION_RELATIONSHIP('SRR','None',#5491,#216);
#195=SHAPE_REPRESENTATION_RELATIONSHIP('SRR','None',#5493,#217);
#196=SHAPE_REPRESENTATION_RELATIONSHIP('SRR','None',#5494,#218);
#197=SHAPE_REPRESENTATION_RELATIONSHIP('SRR','None',#5495,#219);
#198=SHAPE_REPRESENTATION_RELATIONSHIP('SRR','None',#5496,#220);
#199=SHAPE_REPRESENTATION_RELATIONSHIP('SRR','None',#5497,#221);
#200=ADVANCED_BREP_SHAPE_REPRESENTATION('',(#252),#5360);
#201=ADVANCED_BREP_SHAPE_REPRESENTATION('',(#253),#5361);
#202=ADVANCED_BREP_SHAPE_REPRESENTATION('',(#254),#5362);
#203=ADVANCED_BREP_SHAPE_REPRESENTATION('',(#255),#5363);
#204=ADVANCED_BREP_SHAPE_REPRESENTATION('',(#256),#5364);
#205=ADVANCED_BREP_SHAPE_REPRESENTATION('',(#257),#5366);
#206=ADVANCED_BREP_SHAPE_REPRESENTATION('',(#258),#5367);
#207=ADVANCED_BREP_SHAPE_REPRESENTATION('',(#259),#5368);
#208=ADVANCED_BREP_SHAPE_REPRESENTATION('',(#260),#5369);
#209=ADVANCED_BREP_SHAPE_REPRESENTATION('',(#261),#5370);
#210=ADVANCED_BREP_SHAPE_REPRESENTATION('',(#262),#5371);
#211=ADVANCED_BREP_SHAPE_REPRESENTATION('',(#263),#5372);
#212=ADVANCED_BREP_SHAPE_REPRESENTATION('',(#264),#5373);
#213=ADVANCED_BREP_SHAPE_REPRESENTATION('',(#48),#5374);
#214=ADVANCED_BREP_SHAPE_REPRESENTATION('',(#265),#5376);
#215=ADVANCED_BREP_SHAPE_REPRESENTATION('',(#266),#5377);
#216=ADVANCED_BREP_SHAPE_REPRESENTATION('',(#267),#5378);
#217=ADVANCED_BREP_SHAPE_REPRESENTATION('',(#268),#5380);
#218=ADVANCED_BREP_SHAPE_REPRESENTATION('',(#269),#5381);
#219=ADVANCED_BREP_SHAPE_REPRESENTATION('',(#270,#271,#272,#273,#274,#275,
#276,#277),#5382);
#220=ADVANCED_BREP_SHAPE_REPRESENTATION('',(#278),#5383);
#221=ADVANCED_BREP_SHAPE_REPRESENTATION('',(#279,#280),#5384);
#222=STYLED_ITEM('',(#5658),#252);
#223=STYLED_ITEM('',(#5672),#253);
#224=STYLED_ITEM('',(#5658),#254);
#225=STYLED_ITEM('',(#5679),#255);
#226=STYLED_ITEM('',(#5679),#256);
#227=STYLED_ITEM('',(#5686),#257);
#228=STYLED_ITEM('',(#5665),#258);
#229=STYLED_ITEM('',(#5665),#259);
#230=STYLED_ITEM('',(#5686),#260);
#231=STYLED_ITEM('',(#5672),#261);
#232=STYLED_ITEM('',(#5672),#262);
#233=STYLED_ITEM('',(#5672),#263);
#234=STYLED_ITEM('',(#5672),#264);
#235=STYLED_ITEM('',(#5679),#48);
#236=STYLED_ITEM('',(#5686),#265);
#237=STYLED_ITEM('',(#5672),#266);
#238=STYLED_ITEM('',(#5672),#267);
#239=STYLED_ITEM('',(#5672),#268);
#240=STYLED_ITEM('',(#5672),#269);
#241=STYLED_ITEM('',(#5672),#270);
#242=STYLED_ITEM('',(#5672),#271);
#243=STYLED_ITEM('',(#5672),#272);
#244=STYLED_ITEM('',(#5672),#273);
#245=STYLED_ITEM('',(#5672),#274);
#246=STYLED_ITEM('',(#5672),#275);
#247=STYLED_ITEM('',(#5672),#276);
#248=STYLED_ITEM('',(#5672),#277);
#249=STYLED_ITEM('',(#5672),#278);
#250=STYLED_ITEM('',(#5672),#279);
#251=STYLED_ITEM('',(#5672),#280);
#252=MANIFOLD_SOLID_BREP('Body1',#2649);
#253=MANIFOLD_SOLID_BREP('Body1',#2650);
#254=MANIFOLD_SOLID_BREP('Body1',#2651);
#255=MANIFOLD_SOLID_BREP('Body1',#2652);
#256=MANIFOLD_SOLID_BREP('Body1',#2653);
#257=MANIFOLD_SOLID_BREP('Body1',#2654);
#258=MANIFOLD_SOLID_BREP('Body1',#2655);
#259=MANIFOLD_SOLID_BREP('Body1',#2656);
#260=MANIFOLD_SOLID_BREP('Body1',#2657);
#261=MANIFOLD_SOLID_BREP('Body1',#2658);
#262=MANIFOLD_SOLID_BREP('Body1',#2659);
#263=MANIFOLD_SOLID_BREP('Body1',#2660);
#264=MANIFOLD_SOLID_BREP('Body1',#2661);
#265=MANIFOLD_SOLID_BREP('Body1',#2664);
#266=MANIFOLD_SOLID_BREP('Body1',#2665);
#267=MANIFOLD_SOLID_BREP('Body1',#2666);
#268=MANIFOLD_SOLID_BREP('Body1',#2667);
#269=MANIFOLD_SOLID_BREP('Body1',#2668);
#270=MANIFOLD_SOLID_BREP('Body1',#2669);
#271=MANIFOLD_SOLID_BREP('Body2',#2670);
#272=MANIFOLD_SOLID_BREP('Body3',#2671);
#273=MANIFOLD_SOLID_BREP('Body4',#2672);
#274=MANIFOLD_SOLID_BREP('Body5',#2673);
#275=MANIFOLD_SOLID_BREP('Body6',#2674);
#276=MANIFOLD_SOLID_BREP('Body7',#2675);
#277=MANIFOLD_SOLID_BREP('Body8',#2676);
#278=MANIFOLD_SOLID_BREP('Continuous crown cage',#2677);
#279=MANIFOLD_SOLID_BREP('Body1',#2678);
#280=MANIFOLD_SOLID_BREP('Body2',#2679);
#281=FACE_BOUND('',#599,.T.);
#282=FACE_BOUND('',#600,.T.);
#283=FACE_BOUND('',#601,.T.);
#284=FACE_BOUND('',#602,.T.);
#285=FACE_BOUND('',#603,.T.);
#286=FACE_BOUND('',#605,.T.);
#287=FACE_BOUND('',#606,.T.);
#288=FACE_BOUND('',#607,.T.);
#289=FACE_BOUND('',#608,.T.);
#290=FACE_BOUND('',#609,.T.);
#291=FACE_BOUND('',#613,.T.);
#292=FACE_BOUND('',#618,.T.);
#293=FACE_BOUND('',#622,.T.);
#294=FACE_BOUND('',#624,.T.);
#295=FACE_BOUND('',#628,.T.);
#296=FACE_BOUND('',#630,.T.);
#297=FACE_BOUND('',#641,.T.);
#298=FACE_BOUND('',#643,.T.);
#299=FACE_BOUND('',#655,.T.);
#300=FACE_BOUND('',#662,.T.);
#301=FACE_BOUND('',#666,.T.);
#302=FACE_BOUND('',#668,.T.);
#303=FACE_BOUND('',#672,.T.);
#304=FACE_BOUND('',#674,.T.);
#305=FACE_BOUND('',#678,.T.);
#306=FACE_BOUND('',#680,.T.);
#307=FACE_BOUND('',#684,.T.);
#308=FACE_BOUND('',#689,.T.);
#309=FACE_BOUND('',#693,.T.);
#310=FACE_BOUND('',#695,.T.);
#311=FACE_BOUND('',#699,.T.);
#312=FACE_BOUND('',#701,.T.);
#313=FACE_BOUND('',#705,.T.);
#314=FACE_BOUND('',#707,.T.);
#315=FACE_BOUND('',#722,.T.);
#316=FACE_BOUND('',#727,.T.);
#317=FACE_BOUND('',#730,.T.);
#318=FACE_BOUND('',#734,.T.);
#319=FACE_BOUND('',#736,.T.);
#320=FACE_BOUND('',#740,.T.);
#321=FACE_BOUND('',#742,.T.);
#322=FACE_BOUND('',#746,.T.);
#323=FACE_BOUND('',#748,.T.);
#324=FACE_BOUND('',#754,.T.);
#325=FACE_BOUND('',#757,.T.);
#326=FACE_BOUND('',#762,.T.);
#327=FACE_BOUND('',#767,.T.);
#328=FACE_BOUND('',#795,.T.);
#329=FACE_BOUND('',#798,.T.);
#330=FACE_BOUND('',#801,.T.);
#331=FACE_BOUND('',#804,.T.);
#332=FACE_BOUND('',#807,.T.);
#333=PLANE('',#2941);
#334=PLANE('',#2942);
#335=PLANE('',#2943);
#336=PLANE('',#2944);
#337=PLANE('',#2945);
#338=PLANE('',#2946);
#339=PLANE('',#2951);
#340=PLANE('',#2952);
#341=PLANE('',#2957);
#342=PLANE('',#2960);
#343=PLANE('',#2968);
#344=PLANE('',#2969);
#345=PLANE('',#2977);
#346=PLANE('',#2978);
#347=PLANE('',#2984);
#348=PLANE('',#2985);
#349=PLANE('',#2986);
#350=PLANE('',#2990);
#351=PLANE('',#2991);
#352=PLANE('',#2992);
#353=PLANE('',#2993);
#354=PLANE('',#2994);
#355=PLANE('',#3011);
#356=PLANE('',#3012);
#357=PLANE('',#3013);
#358=PLANE('',#3014);
#359=PLANE('',#3015);
#360=PLANE('',#3016);
#361=PLANE('',#3017);
#362=PLANE('',#3018);
#363=PLANE('',#3019);
#364=PLANE('',#3020);
#365=PLANE('',#3021);
#366=PLANE('',#3022);
#367=PLANE('',#3023);
#368=PLANE('',#3024);
#369=PLANE('',#3032);
#370=PLANE('',#3033);
#371=PLANE('',#3041);
#372=PLANE('',#3042);
#373=PLANE('',#3050);
#374=PLANE('',#3051);
#375=PLANE('',#3056);
#376=PLANE('',#3057);
#377=PLANE('',#3062);
#378=PLANE('',#3065);
#379=PLANE('',#3073);
#380=PLANE('',#3074);
#381=PLANE('',#3082);
#382=PLANE('',#3083);
#383=PLANE('',#3091);
#384=PLANE('',#3092);
#385=PLANE('',#3094);
#386=PLANE('',#3095);
#387=PLANE('',#3096);
#388=PLANE('',#3097);
#389=PLANE('',#3098);
#390=PLANE('',#3099);
#391=PLANE('',#3100);
#392=PLANE('',#3101);
#393=PLANE('',#3102);
#394=PLANE('',#3104);
#395=PLANE('',#3112);
#396=PLANE('',#3131);
#397=PLANE('',#3136);
#398=PLANE('',#3142);
#399=PLANE('',#3143);
#400=PLANE('',#3151);
#401=PLANE('',#3152);
#402=PLANE('',#3160);
#403=PLANE('',#3161);
#404=PLANE('',#3177);
#405=PLANE('',#3180);
#406=PLANE('',#3192);
#407=PLANE('',#3201);
#408=PLANE('',#3234);
#409=PLANE('',#3239);
#410=PLANE('',#3244);
#411=PLANE('',#3249);
#412=PLANE('',#3254);
#413=PLANE('',#3259);
#414=PLANE('',#3268);
#415=PLANE('',#3272);
#416=PLANE('',#3273);
#417=PLANE('',#3275);
#418=PLANE('',#3280);
#419=PLANE('',#3283);
#420=PLANE('',#3288);
#421=FACE_OUTER_BOUND('',#589,.T.);
#422=FACE_OUTER_BOUND('',#590,.T.);
#423=FACE_OUTER_BOUND('',#591,.T.);
#424=FACE_OUTER_BOUND('',#592,.T.);
#425=FACE_OUTER_BOUND('',#593,.T.);
#426=FACE_OUTER_BOUND('',#594,.T.);
#427=FACE_OUTER_BOUND('',#595,.T.);
#428=FACE_OUTER_BOUND('',#596,.T.);
#429=FACE_OUTER_BOUND('',#597,.T.);
#430=FACE_OUTER_BOUND('',#598,.T.);
#431=FACE_OUTER_BOUND('',#604,.T.);
#432=FACE_OUTER_BOUND('',#610,.T.);
#433=FACE_OUTER_BOUND('',#611,.T.);
#434=FACE_OUTER_BOUND('',#612,.T.);
#435=FACE_OUTER_BOUND('',#614,.T.);
#436=FACE_OUTER_BOUND('',#615,.T.);
#437=FACE_OUTER_BOUND('',#616,.T.);
#438=FACE_OUTER_BOUND('',#617,.T.);
#439=FACE_OUTER_BOUND('',#619,.T.);
#440=FACE_OUTER_BOUND('',#620,.T.);
#441=FACE_OUTER_BOUND('',#621,.T.);
#442=FACE_OUTER_BOUND('',#623,.T.);
#443=FACE_OUTER_BOUND('',#625,.T.);
#444=FACE_OUTER_BOUND('',#626,.T.);
#445=FACE_OUTER_BOUND('',#627,.T.);
#446=FACE_OUTER_BOUND('',#629,.T.);
#447=FACE_OUTER_BOUND('',#631,.T.);
#448=FACE_OUTER_BOUND('',#632,.T.);
#449=FACE_OUTER_BOUND('',#633,.T.);
#450=FACE_OUTER_BOUND('',#634,.T.);
#451=FACE_OUTER_BOUND('',#635,.T.);
#452=FACE_OUTER_BOUND('',#636,.T.);
#453=FACE_OUTER_BOUND('',#637,.T.);
#454=FACE_OUTER_BOUND('',#638,.T.);
#455=FACE_OUTER_BOUND('',#639,.T.);
#456=FACE_OUTER_BOUND('',#640,.T.);
#457=FACE_OUTER_BOUND('',#642,.T.);
#458=FACE_OUTER_BOUND('',#644,.T.);
#459=FACE_OUTER_BOUND('',#645,.T.);
#460=FACE_OUTER_BOUND('',#646,.T.);
#461=FACE_OUTER_BOUND('',#647,.T.);
#462=FACE_OUTER_BOUND('',#648,.T.);
#463=FACE_OUTER_BOUND('',#649,.T.);
#464=FACE_OUTER_BOUND('',#650,.T.);
#465=FACE_OUTER_BOUND('',#651,.T.);
#466=FACE_OUTER_BOUND('',#652,.T.);
#467=FACE_OUTER_BOUND('',#653,.T.);
#468=FACE_OUTER_BOUND('',#654,.T.);
#469=FACE_OUTER_BOUND('',#656,.T.);
#470=FACE_OUTER_BOUND('',#657,.T.);
#471=FACE_OUTER_BOUND('',#658,.T.);
#472=FACE_OUTER_BOUND('',#659,.T.);
#473=FACE_OUTER_BOUND('',#660,.T.);
#474=FACE_OUTER_BOUND('',#661,.T.);
#475=FACE_OUTER_BOUND('',#663,.T.);
#476=FACE_OUTER_BOUND('',#664,.T.);
#477=FACE_OUTER_BOUND('',#665,.T.);
#478=FACE_OUTER_BOUND('',#667,.T.);
#479=FACE_OUTER_BOUND('',#669,.T.);
#480=FACE_OUTER_BOUND('',#670,.T.);
#481=FACE_OUTER_BOUND('',#671,.T.);
#482=FACE_OUTER_BOUND('',#673,.T.);
#483=FACE_OUTER_BOUND('',#675,.T.);
#484=FACE_OUTER_BOUND('',#676,.T.);
#485=FACE_OUTER_BOUND('',#677,.T.);
#486=FACE_OUTER_BOUND('',#679,.T.);
#487=FACE_OUTER_BOUND('',#681,.T.);
#488=FACE_OUTER_BOUND('',#682,.T.);
#489=FACE_OUTER_BOUND('',#683,.T.);
#490=FACE_OUTER_BOUND('',#685,.T.);
#491=FACE_OUTER_BOUND('',#686,.T.);
#492=FACE_OUTER_BOUND('',#687,.T.);
#493=FACE_OUTER_BOUND('',#688,.T.);
#494=FACE_OUTER_BOUND('',#690,.T.);
#495=FACE_OUTER_BOUND('',#691,.T.);
#496=FACE_OUTER_BOUND('',#692,.T.);
#497=FACE_OUTER_BOUND('',#694,.T.);
#498=FACE_OUTER_BOUND('',#696,.T.);
#499=FACE_OUTER_BOUND('',#697,.T.);
#500=FACE_OUTER_BOUND('',#698,.T.);
#501=FACE_OUTER_BOUND('',#700,.T.);
#502=FACE_OUTER_BOUND('',#702,.T.);
#503=FACE_OUTER_BOUND('',#703,.T.);
#504=FACE_OUTER_BOUND('',#704,.T.);
#505=FACE_OUTER_BOUND('',#706,.T.);
#506=FACE_OUTER_BOUND('',#708,.T.);
#507=FACE_OUTER_BOUND('',#709,.T.);
#508=FACE_OUTER_BOUND('',#710,.T.);
#509=FACE_OUTER_BOUND('',#711,.T.);
#510=FACE_OUTER_BOUND('',#712,.T.);
#511=FACE_OUTER_BOUND('',#713,.T.);
#512=FACE_OUTER_BOUND('',#714,.T.);
#513=FACE_OUTER_BOUND('',#715,.T.);
#514=FACE_OUTER_BOUND('',#716,.T.);
#515=FACE_OUTER_BOUND('',#717,.T.);
#516=FACE_OUTER_BOUND('',#718,.T.);
#517=FACE_OUTER_BOUND('',#719,.T.);
#518=FACE_OUTER_BOUND('',#720,.T.);
#519=FACE_OUTER_BOUND('',#721,.T.);
#520=FACE_OUTER_BOUND('',#723,.T.);
#521=FACE_OUTER_BOUND('',#724,.T.);
#522=FACE_OUTER_BOUND('',#725,.T.);
#523=FACE_OUTER_BOUND('',#726,.T.);
#524=FACE_OUTER_BOUND('',#728,.T.);
#525=FACE_OUTER_BOUND('',#729,.T.);
#526=FACE_OUTER_BOUND('',#731,.T.);
#527=FACE_OUTER_BOUND('',#732,.T.);
#528=FACE_OUTER_BOUND('',#733,.T.);
#529=FACE_OUTER_BOUND('',#735,.T.);
#530=FACE_OUTER_BOUND('',#737,.T.);
#531=FACE_OUTER_BOUND('',#738,.T.);
#532=FACE_OUTER_BOUND('',#739,.T.);
#533=FACE_OUTER_BOUND('',#741,.T.);
#534=FACE_OUTER_BOUND('',#743,.T.);
#535=FACE_OUTER_BOUND('',#744,.T.);
#536=FACE_OUTER_BOUND('',#745,.T.);
#537=FACE_OUTER_BOUND('',#747,.T.);
#538=FACE_OUTER_BOUND('',#749,.T.);
#539=FACE_OUTER_BOUND('',#750,.T.);
#540=FACE_OUTER_BOUND('',#751,.T.);
#541=FACE_OUTER_BOUND('',#752,.T.);
#542=FACE_OUTER_BOUND('',#753,.T.);
#543=FACE_OUTER_BOUND('',#755,.T.);
#544=FACE_OUTER_BOUND('',#756,.T.);
#545=FACE_OUTER_BOUND('',#758,.T.);
#546=FACE_OUTER_BOUND('',#759,.T.);
#547=FACE_OUTER_BOUND('',#760,.T.);
#548=FACE_OUTER_BOUND('',#761,.T.);
#549=FACE_OUTER_BOUND('',#763,.T.);
#550=FACE_OUTER_BOUND('',#764,.T.);
#551=FACE_OUTER_BOUND('',#765,.T.);
#552=FACE_OUTER_BOUND('',#766,.T.);
#553=FACE_OUTER_BOUND('',#768,.T.);
#554=FACE_OUTER_BOUND('',#769,.T.);
#555=FACE_OUTER_BOUND('',#770,.T.);
#556=FACE_OUTER_BOUND('',#771,.T.);
#557=FACE_OUTER_BOUND('',#772,.T.);
#558=FACE_OUTER_BOUND('',#773,.T.);
#559=FACE_OUTER_BOUND('',#774,.T.);
#560=FACE_OUTER_BOUND('',#775,.T.);
#561=FACE_OUTER_BOUND('',#776,.T.);
#562=FACE_OUTER_BOUND('',#777,.T.);
#563=FACE_OUTER_BOUND('',#778,.T.);
#564=FACE_OUTER_BOUND('',#779,.T.);
#565=FACE_OUTER_BOUND('',#780,.T.);
#566=FACE_OUTER_BOUND('',#781,.T.);
#567=FACE_OUTER_BOUND('',#782,.T.);
#568=FACE_OUTER_BOUND('',#783,.T.);
#569=FACE_OUTER_BOUND('',#784,.T.);
#570=FACE_OUTER_BOUND('',#785,.T.);
#571=FACE_OUTER_BOUND('',#786,.T.);
#572=FACE_OUTER_BOUND('',#787,.T.);
#573=FACE_OUTER_BOUND('',#788,.T.);
#574=FACE_OUTER_BOUND('',#789,.T.);
#575=FACE_OUTER_BOUND('',#790,.T.);
#576=FACE_OUTER_BOUND('',#791,.T.);
#577=FACE_OUTER_BOUND('',#792,.T.);
#578=FACE_OUTER_BOUND('',#793,.T.);
#579=FACE_OUTER_BOUND('',#794,.T.);
#580=FACE_OUTER_BOUND('',#796,.T.);
#581=FACE_OUTER_BOUND('',#797,.T.);
#582=FACE_OUTER_BOUND('',#799,.T.);
#583=FACE_OUTER_BOUND('',#800,.T.);
#584=FACE_OUTER_BOUND('',#802,.T.);
#585=FACE_OUTER_BOUND('',#803,.T.);
#586=FACE_OUTER_BOUND('',#805,.T.);
#587=FACE_OUTER_BOUND('',#806,.T.);
#588=FACE_OUTER_BOUND('',#808,.T.);
#589=EDGE_LOOP('',(#1782,#1783,#1784,#1785));
#590=EDGE_LOOP('',(#1786,#1787,#1788,#1789));
#591=EDGE_LOOP('',(#1790,#1791,#1792,#1793));
#592=EDGE_LOOP('',(#1794,#1795,#1796,#1797));
#593=EDGE_LOOP('',(#1798,#1799,#1800,#1801));
#594=EDGE_LOOP('',(#1802,#1803,#1804,#1805));
#595=EDGE_LOOP('',(#1806,#1807,#1808,#1809));
#596=EDGE_LOOP('',(#1810,#1811,#1812,#1813));
#597=EDGE_LOOP('',(#1814,#1815,#1816,#1817));
#598=EDGE_LOOP('',(#1818,#1819,#1820,#1821));
#599=EDGE_LOOP('',(#1822));
#600=EDGE_LOOP('',(#1823));
#601=EDGE_LOOP('',(#1824));
#602=EDGE_LOOP('',(#1825));
#603=EDGE_LOOP('',(#1826));
#604=EDGE_LOOP('',(#1827,#1828,#1829,#1830));
#605=EDGE_LOOP('',(#1831));
#606=EDGE_LOOP('',(#1832));
#607=EDGE_LOOP('',(#1833));
#608=EDGE_LOOP('',(#1834));
#609=EDGE_LOOP('',(#1835));
#610=EDGE_LOOP('',(#1836,#1837,#1838,#1839));
#611=EDGE_LOOP('',(#1840));
#612=EDGE_LOOP('',(#1841));
#613=EDGE_LOOP('',(#1842));
#614=EDGE_LOOP('',(#1843,#1844,#1845,#1846));
#615=EDGE_LOOP('',(#1847));
#616=EDGE_LOOP('',(#1848,#1849,#1850,#1851));
#617=EDGE_LOOP('',(#1852));
#618=EDGE_LOOP('',(#1853));
#619=EDGE_LOOP('',(#1854,#1855,#1856,#1857));
#620=EDGE_LOOP('',(#1858,#1859,#1860,#1861));
#621=EDGE_LOOP('',(#1862));
#622=EDGE_LOOP('',(#1863));
#623=EDGE_LOOP('',(#1864));
#624=EDGE_LOOP('',(#1865));
#625=EDGE_LOOP('',(#1866,#1867,#1868,#1869));
#626=EDGE_LOOP('',(#1870,#1871,#1872,#1873));
#627=EDGE_LOOP('',(#1874));
#628=EDGE_LOOP('',(#1875));
#629=EDGE_LOOP('',(#1876));
#630=EDGE_LOOP('',(#1877));
#631=EDGE_LOOP('',(#1878,#1879,#1880,#1881,#1882,#1883,#1884,#1885,#1886));
#632=EDGE_LOOP('',(#1887,#1888,#1889,#1890,#1891,#1892,#1893,#1894,#1895));
#633=EDGE_LOOP('',(#1896,#1897,#1898,#1899));
#634=EDGE_LOOP('',(#1900,#1901,#1902,#1903));
#635=EDGE_LOOP('',(#1904,#1905,#1906,#1907));
#636=EDGE_LOOP('',(#1908,#1909,#1910,#1911));
#637=EDGE_LOOP('',(#1912,#1913,#1914,#1915));
#638=EDGE_LOOP('',(#1916,#1917,#1918,#1919));
#639=EDGE_LOOP('',(#1920,#1921,#1922,#1923));
#640=EDGE_LOOP('',(#1924));
#641=EDGE_LOOP('',(#1925));
#642=EDGE_LOOP('',(#1926));
#643=EDGE_LOOP('',(#1927));
#644=EDGE_LOOP('',(#1928,#1929,#1930,#1931));
#645=EDGE_LOOP('',(#1932,#1933,#1934,#1935));
#646=EDGE_LOOP('',(#1936,#1937,#1938,#1939));
#647=EDGE_LOOP('',(#1940,#1941,#1942,#1943,#1944,#1945,#1946,#1947));
#648=EDGE_LOOP('',(#1948,#1949,#1950,#1951));
#649=EDGE_LOOP('',(#1952,#1953,#1954,#1955));
#650=EDGE_LOOP('',(#1956,#1957,#1958,#1959,#1960,#1961,#1962,#1963));
#651=EDGE_LOOP('',(#1964,#1965,#1966,#1967));
#652=EDGE_LOOP('',(#1968,#1969,#1970,#1971));
#653=EDGE_LOOP('',(#1972,#1973,#1974,#1975,#1976,#1977));
#654=EDGE_LOOP('',(#1978,#1979,#1980,#1981,#1982,#1983,#1984,#1985));
#655=EDGE_LOOP('',(#1986));
#656=EDGE_LOOP('',(#1987,#1988,#1989,#1990,#1991,#1992,#1993,#1994));
#657=EDGE_LOOP('',(#1995,#1996,#1997,#1998,#1999,#2000));
#658=EDGE_LOOP('',(#2001,#2002,#2003,#2004));
#659=EDGE_LOOP('',(#2005,#2006,#2007,#2008));
#660=EDGE_LOOP('',(#2009,#2010,#2011,#2012));
#661=EDGE_LOOP('',(#2013,#2014,#2015,#2016));
#662=EDGE_LOOP('',(#2017));
#663=EDGE_LOOP('',(#2018,#2019,#2020,#2021));
#664=EDGE_LOOP('',(#2022,#2023,#2024,#2025));
#665=EDGE_LOOP('',(#2026));
#666=EDGE_LOOP('',(#2027));
#667=EDGE_LOOP('',(#2028));
#668=EDGE_LOOP('',(#2029));
#669=EDGE_LOOP('',(#2030,#2031,#2032,#2033));
#670=EDGE_LOOP('',(#2034,#2035,#2036,#2037));
#671=EDGE_LOOP('',(#2038));
#672=EDGE_LOOP('',(#2039));
#673=EDGE_LOOP('',(#2040));
#674=EDGE_LOOP('',(#2041));
#675=EDGE_LOOP('',(#2042,#2043,#2044,#2045));
#676=EDGE_LOOP('',(#2046,#2047,#2048,#2049));
#677=EDGE_LOOP('',(#2050));
#678=EDGE_LOOP('',(#2051));
#679=EDGE_LOOP('',(#2052));
#680=EDGE_LOOP('',(#2053));
#681=EDGE_LOOP('',(#2054,#2055,#2056,#2057));
#682=EDGE_LOOP('',(#2058));
#683=EDGE_LOOP('',(#2059));
#684=EDGE_LOOP('',(#2060));
#685=EDGE_LOOP('',(#2061,#2062,#2063,#2064));
#686=EDGE_LOOP('',(#2065));
#687=EDGE_LOOP('',(#2066,#2067,#2068,#2069));
#688=EDGE_LOOP('',(#2070));
#689=EDGE_LOOP('',(#2071));
#690=EDGE_LOOP('',(#2072,#2073,#2074,#2075));
#691=EDGE_LOOP('',(#2076,#2077,#2078,#2079));
#692=EDGE_LOOP('',(#2080));
#693=EDGE_LOOP('',(#2081));
#694=EDGE_LOOP('',(#2082));
#695=EDGE_LOOP('',(#2083));
#696=EDGE_LOOP('',(#2084,#2085,#2086,#2087));
#697=EDGE_LOOP('',(#2088,#2089,#2090,#2091));
#698=EDGE_LOOP('',(#2092));
#699=EDGE_LOOP('',(#2093));
#700=EDGE_LOOP('',(#2094));
#701=EDGE_LOOP('',(#2095));
#702=EDGE_LOOP('',(#2096,#2097,#2098,#2099));
#703=EDGE_LOOP('',(#2100,#2101,#2102,#2103));
#704=EDGE_LOOP('',(#2104));
#705=EDGE_LOOP('',(#2105));
#706=EDGE_LOOP('',(#2106));
#707=EDGE_LOOP('',(#2107));
#708=EDGE_LOOP('',(#2108,#2109,#2110,#2111));
#709=EDGE_LOOP('',(#2112,#2113,#2114,#2115));
#710=EDGE_LOOP('',(#2116,#2117,#2118,#2119));
#711=EDGE_LOOP('',(#2120,#2121,#2122,#2123));
#712=EDGE_LOOP('',(#2124,#2125,#2126,#2127));
#713=EDGE_LOOP('',(#2128,#2129,#2130,#2131));
#714=EDGE_LOOP('',(#2132,#2133,#2134,#2135,#2136,#2137));
#715=EDGE_LOOP('',(#2138,#2139,#2140,#2141,#2142,#2143));
#716=EDGE_LOOP('',(#2144));
#717=EDGE_LOOP('',(#2145));
#718=EDGE_LOOP('',(#2146,#2147,#2148,#2149));
#719=EDGE_LOOP('',(#2150,#2151,#2152,#2153));
#720=EDGE_LOOP('',(#2154,#2155,#2156,#2157));
#721=EDGE_LOOP('',(#2158));
#722=EDGE_LOOP('',(#2159));
#723=EDGE_LOOP('',(#2160,#2161,#2162,#2163));
#724=EDGE_LOOP('',(#2164,#2165,#2166,#2167));
#725=EDGE_LOOP('',(#2168,#2169,#2170,#2171));
#726=EDGE_LOOP('',(#2172));
#727=EDGE_LOOP('',(#2173));
#728=EDGE_LOOP('',(#2174,#2175,#2176,#2177));
#729=EDGE_LOOP('',(#2178));
#730=EDGE_LOOP('',(#2179));
#731=EDGE_LOOP('',(#2180,#2181,#2182,#2183));
#732=EDGE_LOOP('',(#2184,#2185,#2186,#2187));
#733=EDGE_LOOP('',(#2188));
#734=EDGE_LOOP('',(#2189));
#735=EDGE_LOOP('',(#2190));
#736=EDGE_LOOP('',(#2191));
#737=EDGE_LOOP('',(#2192,#2193,#2194,#2195));
#738=EDGE_LOOP('',(#2196,#2197,#2198,#2199));
#739=EDGE_LOOP('',(#2200));
#740=EDGE_LOOP('',(#2201));
#741=EDGE_LOOP('',(#2202));
#742=EDGE_LOOP('',(#2203));
#743=EDGE_LOOP('',(#2204,#2205,#2206,#2207));
#744=EDGE_LOOP('',(#2208,#2209,#2210,#2211));
#745=EDGE_LOOP('',(#2212));
#746=EDGE_LOOP('',(#2213));
#747=EDGE_LOOP('',(#2214));
#748=EDGE_LOOP('',(#2215));
#749=EDGE_LOOP('',(#2216,#2217,#2218,#2219,#2220,#2221));
#750=EDGE_LOOP('',(#2222,#2223,#2224,#2225,#2226));
#751=EDGE_LOOP('',(#2227,#2228,#2229,#2230));
#752=EDGE_LOOP('',(#2231,#2232,#2233,#2234));
#753=EDGE_LOOP('',(#2235));
#754=EDGE_LOOP('',(#2236));
#755=EDGE_LOOP('',(#2237,#2238,#2239,#2240,#2241));
#756=EDGE_LOOP('',(#2242));
#757=EDGE_LOOP('',(#2243));
#758=EDGE_LOOP('',(#2244,#2245,#2246,#2247));
#759=EDGE_LOOP('',(#2248,#2249,#2250,#2251,#2252,#2253));
#760=EDGE_LOOP('',(#2254,#2255,#2256,#2257,#2258));
#761=EDGE_LOOP('',(#2259));
#762=EDGE_LOOP('',(#2260));
#763=EDGE_LOOP('',(#2261,#2262,#2263,#2264));
#764=EDGE_LOOP('',(#2265,#2266,#2267,#2268));
#765=EDGE_LOOP('',(#2269,#2270,#2271,#2272));
#766=EDGE_LOOP('',(#2273));
#767=EDGE_LOOP('',(#2274));
#768=EDGE_LOOP('',(#2275,#2276,#2277,#2278,#2279));
#769=EDGE_LOOP('',(#2280,#2281));
#770=EDGE_LOOP('',(#2282,#2283));
#771=EDGE_LOOP('',(#2284,#2285));
#772=EDGE_LOOP('',(#2286,#2287));
#773=EDGE_LOOP('',(#2288,#2289));
#774=EDGE_LOOP('',(#2290,#2291));
#775=EDGE_LOOP('',(#2292,#2293));
#776=EDGE_LOOP('',(#2294,#2295));
#777=EDGE_LOOP('',(#2296,#2297,#2298,#2299));
#778=EDGE_LOOP('',(#2300,#2301,#2302,#2303,#2304,#2305,#2306,#2307,#2308,
#2309,#2310,#2311,#2312,#2313,#2314,#2315,#2316,#2317,#2318,#2319));
#779=EDGE_LOOP('',(#2320,#2321,#2322,#2323));
#780=EDGE_LOOP('',(#2324,#2325,#2326,#2327));
#781=EDGE_LOOP('',(#2328,#2329,#2330,#2331));
#782=EDGE_LOOP('',(#2332,#2333,#2334,#2335));
#783=EDGE_LOOP('',(#2336,#2337,#2338,#2339));
#784=EDGE_LOOP('',(#2340,#2341,#2342,#2343,#2344,#2345));
#785=EDGE_LOOP('',(#2346,#2347,#2348,#2349));
#786=EDGE_LOOP('',(#2350,#2351,#2352,#2353));
#787=EDGE_LOOP('',(#2354,#2355,#2356,#2357));
#788=EDGE_LOOP('',(#2358,#2359,#2360,#2361));
#789=EDGE_LOOP('',(#2362,#2363,#2364,#2365));
#790=EDGE_LOOP('',(#2366,#2367,#2368,#2369));
#791=EDGE_LOOP('',(#2370,#2371,#2372,#2373,#2374,#2375,#2376,#2377,#2378,
#2379,#2380,#2381,#2382,#2383,#2384,#2385,#2386,#2387,#2388,#2389));
#792=EDGE_LOOP('',(#2390,#2391,#2392,#2393));
#793=EDGE_LOOP('',(#2394,#2395,#2396,#2397));
#794=EDGE_LOOP('',(#2398));
#795=EDGE_LOOP('',(#2399));
#796=EDGE_LOOP('',(#2400,#2401,#2402,#2403));
#797=EDGE_LOOP('',(#2404));
#798=EDGE_LOOP('',(#2405));
#799=EDGE_LOOP('',(#2406,#2407,#2408,#2409));
#800=EDGE_LOOP('',(#2410));
#801=EDGE_LOOP('',(#2411));
#802=EDGE_LOOP('',(#2412,#2413,#2414,#2415));
#803=EDGE_LOOP('',(#2416));
#804=EDGE_LOOP('',(#2417));
#805=EDGE_LOOP('',(#2418,#2419,#2420,#2421));
#806=EDGE_LOOP('',(#2422));
#807=EDGE_LOOP('',(#2423));
#808=EDGE_LOOP('',(#2424,#2425,#2426,#2427));
#809=LINE('',#4207,#943);
#810=LINE('',#4213,#944);
#811=LINE('',#4219,#945);
#812=LINE('',#4225,#946);
#813=LINE('',#4231,#947);
#814=LINE('',#4236,#948);
#815=LINE('',#4238,#949);
#816=LINE('',#4240,#950);
#817=LINE('',#4241,#951);
#818=LINE('',#4244,#952);
#819=LINE('',#4246,#953);
#820=LINE('',#4247,#954);
#821=LINE('',#4250,#955);
#822=LINE('',#4252,#956);
#823=LINE('',#4253,#957);
#824=LINE('',#4255,#958);
#825=LINE('',#4256,#959);
#826=LINE('',#4264,#960);
#827=LINE('',#4275,#961);
#828=LINE('',#4279,#962);
#829=LINE('',#4287,#963);
#830=LINE('',#4293,#964);
#831=LINE('',#4302,#965);
#832=LINE('',#4308,#966);
#833=LINE('',#4324,#967);
#834=LINE('',#4345,#968);
#835=LINE('',#4370,#969);
#836=LINE('',#4371,#970);
#837=LINE('',#4373,#971);
#838=LINE('',#4375,#972);
#839=LINE('',#4380,#973);
#840=LINE('',#4383,#974);
#841=LINE('',#4385,#975);
#842=LINE('',#4400,#976);
#843=LINE('',#4407,#977);
#844=LINE('',#4410,#978);
#845=LINE('',#4414,#979);
#846=LINE('',#4418,#980);
#847=LINE('',#4422,#981);
#848=LINE('',#4424,#982);
#849=LINE('',#4426,#983);
#850=LINE('',#4428,#984);
#851=LINE('',#4430,#985);
#852=LINE('',#4432,#986);
#853=LINE('',#4433,#987);
#854=LINE('',#4436,#988);
#855=LINE('',#4437,#989);
#856=LINE('',#4440,#990);
#857=LINE('',#4441,#991);
#858=LINE('',#4444,#992);
#859=LINE('',#4446,#993);
#860=LINE('',#4448,#994);
#861=LINE('',#4450,#995);
#862=LINE('',#4452,#996);
#863=LINE('',#4454,#997);
#864=LINE('',#4455,#998);
#865=LINE('',#4458,#999);
#866=LINE('',#4459,#1000);
#867=LINE('',#4462,#1001);
#868=LINE('',#4463,#1002);
#869=LINE('',#4466,#1003);
#870=LINE('',#4467,#1004);
#871=LINE('',#4470,#1005);
#872=LINE('',#4472,#1006);
#873=LINE('',#4473,#1007);
#874=LINE('',#4474,#1008);
#875=LINE('',#4476,#1009);
#876=LINE('',#4477,#1010);
#877=LINE('',#4480,#1011);
#878=LINE('',#4481,#1012);
#879=LINE('',#4483,#1013);
#880=LINE('',#4486,#1014);
#881=LINE('',#4493,#1015);
#882=LINE('',#4499,#1016);
#883=LINE('',#4508,#1017);
#884=LINE('',#4514,#1018);
#885=LINE('',#4523,#1019);
#886=LINE('',#4529,#1020);
#887=LINE('',#4538,#1021);
#888=LINE('',#4548,#1022);
#889=LINE('',#4554,#1023);
#890=LINE('',#4561,#1024);
#891=LINE('',#4567,#1025);
#892=LINE('',#4576,#1026);
#893=LINE('',#4582,#1027);
#894=LINE('',#4591,#1028);
#895=LINE('',#4597,#1029);
#896=LINE('',#4605,#1030);
#897=LINE('',#4607,#1031);
#898=LINE('',#4609,#1032);
#899=LINE('',#4610,#1033);
#900=LINE('',#4613,#1034);
#901=LINE('',#4615,#1035);
#902=LINE('',#4616,#1036);
#903=LINE('',#4619,#1037);
#904=LINE('',#4621,#1038);
#905=LINE('',#4622,#1039);
#906=LINE('',#4625,#1040);
#907=LINE('',#4627,#1041);
#908=LINE('',#4628,#1042);
#909=LINE('',#4631,#1043);
#910=LINE('',#4633,#1044);
#911=LINE('',#4634,#1045);
#912=LINE('',#4636,#1046);
#913=LINE('',#4637,#1047);
#914=LINE('',#4649,#1048);
#915=LINE('',#4653,#1049);
#916=LINE('',#4657,#1050);
#917=LINE('',#4664,#1051);
#918=LINE('',#4666,#1052);
#919=LINE('',#4682,#1053);
#920=LINE('',#4691,#1054);
#921=LINE('',#4697,#1055);
#922=LINE('',#4702,#1056);
#923=LINE('',#4711,#1057);
#924=LINE('',#4717,#1058);
#925=LINE('',#4726,#1059);
#926=LINE('',#4732,#1060);
#927=LINE('',#4750,#1061);
#928=LINE('',#4756,#1062);
#929=LINE('',#4760,#1063);
#930=LINE('',#4766,#1064);
#931=LINE('',#4771,#1065);
#932=LINE('',#4786,#1066);
#933=LINE('',#4795,#1067);
#934=LINE('',#4799,#1068);
#935=LINE('',#4803,#1069);
#936=LINE('',#4806,#1070);
#937=LINE('',#4959,#1071);
#938=LINE('',#5255,#1072);
#939=LINE('',#5297,#1073);
#940=LINE('',#5302,#1074);
#941=LINE('',#5311,#1075);
#942=LINE('',#5316,#1076);
#943=VECTOR('',#3314,0.6);
#944=VECTOR('',#3321,0.425);
#945=VECTOR('',#3328,0.425);
#946=VECTOR('',#3335,0.425);
#947=VECTOR('',#3342,0.425);
#948=VECTOR('',#3347,1.);
#949=VECTOR('',#3348,1.);
#950=VECTOR('',#3349,1.);
#951=VECTOR('',#3350,1.);
#952=VECTOR('',#3353,1.);
#953=VECTOR('',#3354,1.);
#954=VECTOR('',#3355,1.);
#955=VECTOR('',#3358,1.);
#956=VECTOR('',#3359,1.);
#957=VECTOR('',#3360,1.);
#958=VECTOR('',#3363,1.);
#959=VECTOR('',#3364,1.);
#960=VECTOR('',#3375,0.4);
#961=VECTOR('',#3390,1.);
#962=VECTOR('',#3395,0.6);
#963=VECTOR('',#3406,0.605);
#964=VECTOR('',#3413,2.);
#965=VECTOR('',#3426,0.42);
#966=VECTOR('',#3433,0.8);
#967=VECTOR('',#3444,0.734027674973257);
#968=VECTOR('',#3451,0.734027674973257);
#969=VECTOR('',#3454,1.);
#970=VECTOR('',#3455,1.);
#971=VECTOR('',#3458,1.);
#972=VECTOR('',#3461,1.);
#973=VECTOR('',#3466,0.4);
#974=VECTOR('',#3471,1.);
#975=VECTOR('',#3474,1.);
#976=VECTOR('',#3499,0.8);
#977=VECTOR('',#3506,1.);
#978=VECTOR('',#3509,1.);
#979=VECTOR('',#3512,1.);
#980=VECTOR('',#3515,1.);
#981=VECTOR('',#3520,1.);
#982=VECTOR('',#3521,1.);
#983=VECTOR('',#3522,1.);
#984=VECTOR('',#3523,1.);
#985=VECTOR('',#3524,1.);
#986=VECTOR('',#3525,1.);
#987=VECTOR('',#3526,1.);
#988=VECTOR('',#3529,1.);
#989=VECTOR('',#3530,1.);
#990=VECTOR('',#3533,1.);
#991=VECTOR('',#3534,1.);
#992=VECTOR('',#3537,1.);
#993=VECTOR('',#3538,1.);
#994=VECTOR('',#3539,1.);
#995=VECTOR('',#3540,1.);
#996=VECTOR('',#3541,1.);
#997=VECTOR('',#3542,1.);
#998=VECTOR('',#3543,1.);
#999=VECTOR('',#3546,1.);
#1000=VECTOR('',#3547,1.);
#1001=VECTOR('',#3550,1.);
#1002=VECTOR('',#3551,1.);
#1003=VECTOR('',#3554,1.);
#1004=VECTOR('',#3555,1.);
#1005=VECTOR('',#3558,1.);
#1006=VECTOR('',#3559,1.);
#1007=VECTOR('',#3560,1.);
#1008=VECTOR('',#3561,1.);
#1009=VECTOR('',#3564,1.);
#1010=VECTOR('',#3565,1.);
#1011=VECTOR('',#3568,1.);
#1012=VECTOR('',#3569,1.);
#1013=VECTOR('',#3572,1.);
#1014=VECTOR('',#3577,1.);
#1015=VECTOR('',#3586,0.605);
#1016=VECTOR('',#3593,0.8);
#1017=VECTOR('',#3606,0.8);
#1018=VECTOR('',#3613,2.);
#1019=VECTOR('',#3626,2.);
#1020=VECTOR('',#3633,2.2);
#1021=VECTOR('',#3646,0.165);
#1022=VECTOR('',#3659,0.8);
#1023=VECTOR('',#3668,0.5);
#1024=VECTOR('',#3677,0.505);
#1025=VECTOR('',#3684,0.7);
#1026=VECTOR('',#3697,0.505);
#1027=VECTOR('',#3704,0.7);
#1028=VECTOR('',#3717,0.225);
#1029=VECTOR('',#3724,0.8);
#1030=VECTOR('',#3735,1.);
#1031=VECTOR('',#3736,1.);
#1032=VECTOR('',#3737,1.);
#1033=VECTOR('',#3738,1.);
#1034=VECTOR('',#3741,1.);
#1035=VECTOR('',#3742,1.);
#1036=VECTOR('',#3743,1.);
#1037=VECTOR('',#3746,1.);
#1038=VECTOR('',#3747,1.);
#1039=VECTOR('',#3748,1.);
#1040=VECTOR('',#3751,1.);
#1041=VECTOR('',#3752,1.);
#1042=VECTOR('',#3753,1.);
#1043=VECTOR('',#3756,1.);
#1044=VECTOR('',#3757,1.);
#1045=VECTOR('',#3758,1.);
#1046=VECTOR('',#3761,1.);
#1047=VECTOR('',#3762,1.);
#1048=VECTOR('',#3779,0.325);
#1049=VECTOR('',#3784,0.35);
#1050=VECTOR('',#3789,0.335);
#1051=VECTOR('',#3798,0.21);
#1052=VECTOR('',#3801,0.2);
#1053=VECTOR('',#3828,1.5);
#1054=VECTOR('',#3839,1.5);
#1055=VECTOR('',#3848,0.52);
#1056=VECTOR('',#3853,3.75);
#1057=VECTOR('',#3866,1.1);
#1058=VECTOR('',#3873,1.5);
#1059=VECTOR('',#3886,1.1);
#1060=VECTOR('',#3893,1.5);
#1061=VECTOR('',#3918,0.976185);
#1062=VECTOR('',#3925,0.5);
#1063=VECTOR('',#3930,0.53);
#1064=VECTOR('',#3939,0.976185);
#1065=VECTOR('',#3946,0.53);
#1066=VECTOR('',#3965,1.023815);
#1067=VECTOR('',#3976,1.47);
#1068=VECTOR('',#3981,1.5);
#1069=VECTOR('',#3986,1.47);
#1070=VECTOR('',#3991,1.023815);
#1071=VECTOR('',#4042,1.019052);
#1072=VECTOR('',#4119,0.980948);
#1073=VECTOR('',#4148,1.013815);
#1074=VECTOR('',#4155,0.991185);
#1075=VECTOR('',#4166,1.013815);
#1076=VECTOR('',#4173,0.991185);
#1077=CIRCLE('',#2927,0.6);
#1078=CIRCLE('',#2928,0.6);
#1079=CIRCLE('',#2930,0.425);
#1080=CIRCLE('',#2931,0.425);
#1081=CIRCLE('',#2933,0.425);
#1082=CIRCLE('',#2934,0.425);
#1083=CIRCLE('',#2936,0.425);
#1084=CIRCLE('',#2937,0.425);
#1085=CIRCLE('',#2939,0.425);
#1086=CIRCLE('',#2940,0.425);
#1087=CIRCLE('',#2949,0.4);
#1088=CIRCLE('',#2950,0.4);
#1089=CIRCLE('',#2953,1.);
#1090=CIRCLE('',#2954,0.6);
#1091=CIRCLE('',#2956,1.);
#1092=CIRCLE('',#2959,0.6);
#1093=CIRCLE('',#2963,0.605);
#1094=CIRCLE('',#2964,0.605);
#1095=CIRCLE('',#2966,2.);
#1096=CIRCLE('',#2967,2.);
#1097=CIRCLE('',#2972,0.42);
#1098=CIRCLE('',#2973,0.42);
#1099=CIRCLE('',#2975,0.8);
#1100=CIRCLE('',#2976,0.8);
#1101=CIRCLE('',#2981,0.6175);
#1102=CIRCLE('',#2983,0.6175);
#1103=CIRCLE('',#2988,0.338975);
#1104=CIRCLE('',#2989,0.338975);
#1105=CIRCLE('',#3003,0.8);
#1106=CIRCLE('',#3004,0.8);
#1107=CIRCLE('',#3006,0.5);
#1108=CIRCLE('',#3007,0.5);
#1109=CIRCLE('',#3009,0.5);
#1110=CIRCLE('',#3010,0.5);
#1111=CIRCLE('',#3027,0.605);
#1112=CIRCLE('',#3028,0.605);
#1113=CIRCLE('',#3030,0.8);
#1114=CIRCLE('',#3031,0.8);
#1115=CIRCLE('',#3036,0.8);
#1116=CIRCLE('',#3037,0.8);
#1117=CIRCLE('',#3039,2.);
#1118=CIRCLE('',#3040,2.);
#1119=CIRCLE('',#3045,2.);
#1120=CIRCLE('',#3046,2.);
#1121=CIRCLE('',#3048,2.2);
#1122=CIRCLE('',#3049,2.2);
#1123=CIRCLE('',#3054,0.165);
#1124=CIRCLE('',#3055,0.165);
#1125=CIRCLE('',#3058,0.8);
#1126=CIRCLE('',#3059,0.5);
#1127=CIRCLE('',#3061,0.8);
#1128=CIRCLE('',#3064,0.5);
#1129=CIRCLE('',#3068,0.505);
#1130=CIRCLE('',#3069,0.505);
#1131=CIRCLE('',#3071,0.7);
#1132=CIRCLE('',#3072,0.7);
#1133=CIRCLE('',#3077,0.505);
#1134=CIRCLE('',#3078,0.505);
#1135=CIRCLE('',#3080,0.7);
#1136=CIRCLE('',#3081,0.7);
#1137=CIRCLE('',#3086,0.225);
#1138=CIRCLE('',#3087,0.225);
#1139=CIRCLE('',#3089,0.8);
#1140=CIRCLE('',#3090,0.8);
#1141=CIRCLE('',#3103,0.1954);
#1142=CIRCLE('',#3105,0.3);
#1143=CIRCLE('',#3107,0.35);
#1144=CIRCLE('',#3109,0.35);
#1145=CIRCLE('',#3111,0.32);
#1146=CIRCLE('',#3113,0.22);
#1147=CIRCLE('',#3115,0.1954);
#1148=CIRCLE('',#3129,1.5);
#1149=CIRCLE('',#3130,1.5);
#1150=CIRCLE('',#3132,0.52);
#1151=CIRCLE('',#3134,1.5);
#1152=CIRCLE('',#3135,1.5);
#1153=CIRCLE('',#3137,0.52);
#1154=CIRCLE('',#3140,3.75);
#1155=CIRCLE('',#3141,3.75);
#1156=CIRCLE('',#3146,1.1);
#1157=CIRCLE('',#3147,1.1);
#1158=CIRCLE('',#3149,1.5);
#1159=CIRCLE('',#3150,1.5);
#1160=CIRCLE('',#3155,1.1);
#1161=CIRCLE('',#3156,1.1);
#1162=CIRCLE('',#3158,1.5);
#1163=CIRCLE('',#3159,1.5);
#1164=CIRCLE('',#3165,0.976185);
#1165=CIRCLE('',#3166,0.976185);
#1166=CIRCLE('',#3167,0.247676);
#1167=CIRCLE('',#3168,0.976185);
#1168=CIRCLE('',#3169,0.976185);
#1169=CIRCLE('',#3171,0.976185);
#1170=CIRCLE('',#3173,0.5);
#1171=CIRCLE('',#3174,0.5);
#1172=CIRCLE('',#3176,0.56);
#1173=CIRCLE('',#3179,0.976185);
#1174=CIRCLE('',#3181,0.56);
#1175=CIRCLE('',#3185,1.023815);
#1176=CIRCLE('',#3186,1.023815);
#1177=CIRCLE('',#3187,0.247676);
#1178=CIRCLE('',#3188,1.023815);
#1179=CIRCLE('',#3189,1.023815);
#1180=CIRCLE('',#3191,1.023815);
#1181=CIRCLE('',#3193,1.44);
#1182=CIRCLE('',#3194,1.023815);
#1183=CIRCLE('',#3196,1.5);
#1184=CIRCLE('',#3198,1.5);
#1185=CIRCLE('',#3200,1.44);
#1186=CIRCLE('',#3205,0.23815);
#1187=CIRCLE('',#3207,0.23815);
#1188=CIRCLE('',#3209,0.23815);
#1189=CIRCLE('',#3211,0.23815);
#1190=CIRCLE('',#3213,0.23815);
#1191=CIRCLE('',#3215,0.23815);
#1192=CIRCLE('',#3217,0.23815);
#1193=CIRCLE('',#3219,0.23815);
#1194=CIRCLE('',#3222,0.243053047864041);
#1195=CIRCLE('',#3223,0.243053047864041);
#1196=CIRCLE('',#3225,1.019052);
#1197=CIRCLE('',#3226,1.019052);
#1198=CIRCLE('',#3227,1.019052);
#1199=CIRCLE('',#3228,1.019052);
#1200=CIRCLE('',#3229,1.019052);
#1201=CIRCLE('',#3230,1.019052);
#1202=CIRCLE('',#3231,1.019052);
#1203=CIRCLE('',#3232,1.019052);
#1204=CIRCLE('',#3233,1.019052);
#1205=CIRCLE('',#3235,0.980948);
#1206=CIRCLE('',#3236,0.243053047864041);
#1207=CIRCLE('',#3238,0.243053047864041);
#1208=CIRCLE('',#3240,0.980948);
#1209=CIRCLE('',#3241,0.243053047864041);
#1210=CIRCLE('',#3243,0.243053047864041);
#1211=CIRCLE('',#3245,0.980948);
#1212=CIRCLE('',#3246,0.243053047864041);
#1213=CIRCLE('',#3248,0.243053047864041);
#1214=CIRCLE('',#3250,0.980948);
#1215=CIRCLE('',#3251,0.243053047864041);
#1216=CIRCLE('',#3253,0.243053047864041);
#1217=CIRCLE('',#3255,0.980948);
#1218=CIRCLE('',#3256,0.243053047864041);
#1219=CIRCLE('',#3258,0.243053047864041);
#1220=CIRCLE('',#3260,0.980948);
#1221=CIRCLE('',#3261,0.243053047864041);
#1222=CIRCLE('',#3263,0.243053047864041);
#1223=CIRCLE('',#3265,0.980948);
#1224=CIRCLE('',#3266,0.980948);
#1225=CIRCLE('',#3267,0.980948);
#1226=CIRCLE('',#3269,0.243053047864041);
#1227=CIRCLE('',#3271,0.243053047864041);
#1228=CIRCLE('',#3276,1.013815);
#1229=CIRCLE('',#3277,0.991185);
#1230=CIRCLE('',#3279,1.013815);
#1231=CIRCLE('',#3281,0.991185);
#1232=CIRCLE('',#3284,1.013815);
#1233=CIRCLE('',#3285,0.991185);
#1234=CIRCLE('',#3287,1.013815);
#1235=CIRCLE('',#3289,0.991185);
#1236=VERTEX_POINT('',#4204);
#1237=VERTEX_POINT('',#4206);
#1238=VERTEX_POINT('',#4210);
#1239=VERTEX_POINT('',#4212);
#1240=VERTEX_POINT('',#4216);
#1241=VERTEX_POINT('',#4218);
#1242=VERTEX_POINT('',#4222);
#1243=VERTEX_POINT('',#4224);
#1244=VERTEX_POINT('',#4228);
#1245=VERTEX_POINT('',#4230);
#1246=VERTEX_POINT('',#4234);
#1247=VERTEX_POINT('',#4235);
#1248=VERTEX_POINT('',#4237);
#1249=VERTEX_POINT('',#4239);
#1250=VERTEX_POINT('',#4243);
#1251=VERTEX_POINT('',#4245);
#1252=VERTEX_POINT('',#4249);
#1253=VERTEX_POINT('',#4251);
#1254=VERTEX_POINT('',#4261);
#1255=VERTEX_POINT('',#4263);
#1256=VERTEX_POINT('',#4268);
#1257=VERTEX_POINT('',#4270);
#1258=VERTEX_POINT('',#4273);
#1259=VERTEX_POINT('',#4278);
#1260=VERTEX_POINT('',#4284);
#1261=VERTEX_POINT('',#4286);
#1262=VERTEX_POINT('',#4290);
#1263=VERTEX_POINT('',#4292);
#1264=VERTEX_POINT('',#4299);
#1265=VERTEX_POINT('',#4301);
#1266=VERTEX_POINT('',#4305);
#1267=VERTEX_POINT('',#4307);
#1268=VERTEX_POINT('',#4314);
#1269=VERTEX_POINT('',#4315);
#1270=VERTEX_POINT('',#4319);
#1271=VERTEX_POINT('',#4323);
#1272=VERTEX_POINT('',#4326);
#1273=VERTEX_POINT('',#4330);
#1274=VERTEX_POINT('',#4334);
#1275=VERTEX_POINT('',#4342);
#1276=VERTEX_POINT('',#4344);
#1277=VERTEX_POINT('',#4346);
#1278=VERTEX_POINT('',#4350);
#1279=VERTEX_POINT('',#4354);
#1280=VERTEX_POINT('',#4358);
#1281=VERTEX_POINT('',#4362);
#1282=VERTEX_POINT('',#4377);
#1283=VERTEX_POINT('',#4379);
#1284=VERTEX_POINT('',#4397);
#1285=VERTEX_POINT('',#4399);
#1286=VERTEX_POINT('',#4403);
#1287=VERTEX_POINT('',#4404);
#1288=VERTEX_POINT('',#4406);
#1289=VERTEX_POINT('',#4408);
#1290=VERTEX_POINT('',#4412);
#1291=VERTEX_POINT('',#4413);
#1292=VERTEX_POINT('',#4415);
#1293=VERTEX_POINT('',#4417);
#1294=VERTEX_POINT('',#4421);
#1295=VERTEX_POINT('',#4423);
#1296=VERTEX_POINT('',#4425);
#1297=VERTEX_POINT('',#4427);
#1298=VERTEX_POINT('',#4429);
#1299=VERTEX_POINT('',#4431);
#1300=VERTEX_POINT('',#4435);
#1301=VERTEX_POINT('',#4439);
#1302=VERTEX_POINT('',#4443);
#1303=VERTEX_POINT('',#4445);
#1304=VERTEX_POINT('',#4447);
#1305=VERTEX_POINT('',#4449);
#1306=VERTEX_POINT('',#4451);
#1307=VERTEX_POINT('',#4453);
#1308=VERTEX_POINT('',#4457);
#1309=VERTEX_POINT('',#4461);
#1310=VERTEX_POINT('',#4465);
#1311=VERTEX_POINT('',#4469);
#1312=VERTEX_POINT('',#4471);
#1313=VERTEX_POINT('',#4479);
#1314=VERTEX_POINT('',#4490);
#1315=VERTEX_POINT('',#4492);
#1316=VERTEX_POINT('',#4496);
#1317=VERTEX_POINT('',#4498);
#1318=VERTEX_POINT('',#4505);
#1319=VERTEX_POINT('',#4507);
#1320=VERTEX_POINT('',#4511);
#1321=VERTEX_POINT('',#4513);
#1322=VERTEX_POINT('',#4520);
#1323=VERTEX_POINT('',#4522);
#1324=VERTEX_POINT('',#4526);
#1325=VERTEX_POINT('',#4528);
#1326=VERTEX_POINT('',#4535);
#1327=VERTEX_POINT('',#4537);
#1328=VERTEX_POINT('',#4542);
#1329=VERTEX_POINT('',#4544);
#1330=VERTEX_POINT('',#4547);
#1331=VERTEX_POINT('',#4552);
#1332=VERTEX_POINT('',#4558);
#1333=VERTEX_POINT('',#4560);
#1334=VERTEX_POINT('',#4564);
#1335=VERTEX_POINT('',#4566);
#1336=VERTEX_POINT('',#4573);
#1337=VERTEX_POINT('',#4575);
#1338=VERTEX_POINT('',#4579);
#1339=VERTEX_POINT('',#4581);
#1340=VERTEX_POINT('',#4588);
#1341=VERTEX_POINT('',#4590);
#1342=VERTEX_POINT('',#4594);
#1343=VERTEX_POINT('',#4596);
#1344=VERTEX_POINT('',#4603);
#1345=VERTEX_POINT('',#4604);
#1346=VERTEX_POINT('',#4606);
#1347=VERTEX_POINT('',#4608);
#1348=VERTEX_POINT('',#4612);
#1349=VERTEX_POINT('',#4614);
#1350=VERTEX_POINT('',#4618);
#1351=VERTEX_POINT('',#4620);
#1352=VERTEX_POINT('',#4624);
#1353=VERTEX_POINT('',#4626);
#1354=VERTEX_POINT('',#4630);
#1355=VERTEX_POINT('',#4632);
#1356=VERTEX_POINT('',#4641);
#1357=VERTEX_POINT('',#4644);
#1358=VERTEX_POINT('',#4647);
#1359=VERTEX_POINT('',#4651);
#1360=VERTEX_POINT('',#4655);
#1361=VERTEX_POINT('',#4659);
#1362=VERTEX_POINT('',#4662);
#1363=VERTEX_POINT('',#4679);
#1364=VERTEX_POINT('',#4681);
#1365=VERTEX_POINT('',#4685);
#1366=VERTEX_POINT('',#4688);
#1367=VERTEX_POINT('',#4690);
#1368=VERTEX_POINT('',#4694);
#1369=VERTEX_POINT('',#4699);
#1370=VERTEX_POINT('',#4701);
#1371=VERTEX_POINT('',#4708);
#1372=VERTEX_POINT('',#4710);
#1373=VERTEX_POINT('',#4714);
#1374=VERTEX_POINT('',#4716);
#1375=VERTEX_POINT('',#4723);
#1376=VERTEX_POINT('',#4725);
#1377=VERTEX_POINT('',#4729);
#1378=VERTEX_POINT('',#4731);
#1379=VERTEX_POINT('',#4739);
#1380=VERTEX_POINT('',#4740);
#1381=VERTEX_POINT('',#4743);
#1382=VERTEX_POINT('',#4745);
#1383=VERTEX_POINT('',#4749);
#1384=VERTEX_POINT('',#4753);
#1385=VERTEX_POINT('',#4755);
#1386=VERTEX_POINT('',#4759);
#1387=VERTEX_POINT('',#4764);
#1388=VERTEX_POINT('',#4768);
#1389=VERTEX_POINT('',#4774);
#1390=VERTEX_POINT('',#4775);
#1391=VERTEX_POINT('',#4778);
#1392=VERTEX_POINT('',#4780);
#1393=VERTEX_POINT('',#4784);
#1394=VERTEX_POINT('',#4788);
#1395=VERTEX_POINT('',#4790);
#1396=VERTEX_POINT('',#4793);
#1397=VERTEX_POINT('',#4797);
#1398=VERTEX_POINT('',#4801);
#1399=VERTEX_POINT('',#4809);
#1400=VERTEX_POINT('',#4810);
#1401=VERTEX_POINT('',#4813);
#1402=VERTEX_POINT('',#4814);
#1403=VERTEX_POINT('',#4817);
#1404=VERTEX_POINT('',#4818);
#1405=VERTEX_POINT('',#4821);
#1406=VERTEX_POINT('',#4822);
#1407=VERTEX_POINT('',#4825);
#1408=VERTEX_POINT('',#4826);
#1409=VERTEX_POINT('',#4829);
#1410=VERTEX_POINT('',#4830);
#1411=VERTEX_POINT('',#4833);
#1412=VERTEX_POINT('',#4834);
#1413=VERTEX_POINT('',#4837);
#1414=VERTEX_POINT('',#4838);
#1415=VERTEX_POINT('',#4842);
#1416=VERTEX_POINT('',#4843);
#1417=VERTEX_POINT('',#4866);
#1418=VERTEX_POINT('',#4868);
#1419=VERTEX_POINT('',#4893);
#1420=VERTEX_POINT('',#4895);
#1421=VERTEX_POINT('',#4918);
#1422=VERTEX_POINT('',#4920);
#1423=VERTEX_POINT('',#4943);
#1424=VERTEX_POINT('',#4945);
#1425=VERTEX_POINT('',#4958);
#1426=VERTEX_POINT('',#4961);
#1427=VERTEX_POINT('',#4974);
#1428=VERTEX_POINT('',#4976);
#1429=VERTEX_POINT('',#4999);
#1430=VERTEX_POINT('',#5001);
#1431=VERTEX_POINT('',#5024);
#1432=VERTEX_POINT('',#5026);
#1433=VERTEX_POINT('',#5049);
#1434=VERTEX_POINT('',#5051);
#1435=VERTEX_POINT('',#5076);
#1436=VERTEX_POINT('',#5080);
#1437=VERTEX_POINT('',#5105);
#1438=VERTEX_POINT('',#5109);
#1439=VERTEX_POINT('',#5134);
#1440=VERTEX_POINT('',#5138);
#1441=VERTEX_POINT('',#5139);
#1442=VERTEX_POINT('',#5166);
#1443=VERTEX_POINT('',#5170);
#1444=VERTEX_POINT('',#5195);
#1445=VERTEX_POINT('',#5199);
#1446=VERTEX_POINT('',#5224);
#1447=VERTEX_POINT('',#5228);
#1448=VERTEX_POINT('',#5253);
#1449=VERTEX_POINT('',#5256);
#1450=VERTEX_POINT('',#5258);
#1451=VERTEX_POINT('',#5290);
#1452=VERTEX_POINT('',#5292);
#1453=VERTEX_POINT('',#5295);
#1454=VERTEX_POINT('',#5299);
#1455=VERTEX_POINT('',#5304);
#1456=VERTEX_POINT('',#5306);
#1457=VERTEX_POINT('',#5309);
#1458=VERTEX_POINT('',#5313);
#1459=EDGE_CURVE('',#1236,#1236,#1077,.T.);
#1460=EDGE_CURVE('',#1236,#1237,#809,.T.);
#1461=EDGE_CURVE('',#1237,#1237,#1078,.T.);
#1462=EDGE_CURVE('',#1238,#1238,#1079,.T.);
#1463=EDGE_CURVE('',#1238,#1239,#810,.T.);
#1464=EDGE_CURVE('',#1239,#1239,#1080,.T.);
#1465=EDGE_CURVE('',#1240,#1240,#1081,.T.);
#1466=EDGE_CURVE('',#1240,#1241,#811,.T.);
#1467=EDGE_CURVE('',#1241,#1241,#1082,.T.);
#1468=EDGE_CURVE('',#1242,#1242,#1083,.T.);
#1469=EDGE_CURVE('',#1242,#1243,#812,.T.);
#1470=EDGE_CURVE('',#1243,#1243,#1084,.T.);
#1471=EDGE_CURVE('',#1244,#1244,#1085,.T.);
#1472=EDGE_CURVE('',#1244,#1245,#813,.T.);
#1473=EDGE_CURVE('',#1245,#1245,#1086,.T.);
#1474=EDGE_CURVE('',#1246,#1247,#814,.T.);
#1475=EDGE_CURVE('',#1247,#1248,#815,.T.);
#1476=EDGE_CURVE('',#1249,#1248,#816,.T.);
#1477=EDGE_CURVE('',#1246,#1249,#817,.T.);
#1478=EDGE_CURVE('',#1250,#1246,#818,.T.);
#1479=EDGE_CURVE('',#1251,#1249,#819,.T.);
#1480=EDGE_CURVE('',#1250,#1251,#820,.T.);
#1481=EDGE_CURVE('',#1252,#1250,#821,.T.);
#1482=EDGE_CURVE('',#1253,#1251,#822,.T.);
#1483=EDGE_CURVE('',#1252,#1253,#823,.T.);
#1484=EDGE_CURVE('',#1247,#1252,#824,.T.);
#1485=EDGE_CURVE('',#1248,#1253,#825,.T.);
#1486=EDGE_CURVE('',#1254,#1254,#1087,.T.);
#1487=EDGE_CURVE('',#1254,#1255,#826,.T.);
#1488=EDGE_CURVE('',#1255,#1255,#1088,.T.);
#1489=EDGE_CURVE('',#1256,#1256,#1089,.T.);
#1490=EDGE_CURVE('',#1257,#1257,#1090,.T.);
#1491=EDGE_CURVE('',#1258,#1258,#1091,.T.);
#1492=EDGE_CURVE('',#1258,#1256,#827,.T.);
#1493=EDGE_CURVE('',#1257,#1259,#828,.T.);
#1494=EDGE_CURVE('',#1259,#1259,#1092,.T.);
#1495=EDGE_CURVE('',#1260,#1260,#1093,.T.);
#1496=EDGE_CURVE('',#1260,#1261,#829,.T.);
#1497=EDGE_CURVE('',#1261,#1261,#1094,.T.);
#1498=EDGE_CURVE('',#1262,#1262,#1095,.T.);
#1499=EDGE_CURVE('',#1262,#1263,#830,.T.);
#1500=EDGE_CURVE('',#1263,#1263,#1096,.T.);
#1501=EDGE_CURVE('',#1264,#1264,#1097,.T.);
#1502=EDGE_CURVE('',#1264,#1265,#831,.T.);
#1503=EDGE_CURVE('',#1265,#1265,#1098,.T.);
#1504=EDGE_CURVE('',#1266,#1266,#1099,.T.);
#1505=EDGE_CURVE('',#1266,#1267,#832,.T.);
#1506=EDGE_CURVE('',#1267,#1267,#1100,.T.);
#1507=EDGE_CURVE('',#1268,#1269,#157,.T.);
#1508=EDGE_CURVE('',#1270,#1268,#158,.T.);
#1509=EDGE_CURVE('',#1270,#1271,#833,.T.);
#1510=EDGE_CURVE('',#1271,#1271,#1101,.T.);
#1511=EDGE_CURVE('',#1272,#1270,#159,.T.);
#1512=EDGE_CURVE('',#1273,#1272,#160,.T.);
#1513=EDGE_CURVE('',#1274,#1273,#161,.T.);
#1514=EDGE_CURVE('',#1269,#1274,#162,.T.);
#1515=EDGE_CURVE('',#1275,#1275,#1102,.T.);
#1516=EDGE_CURVE('',#1275,#1276,#834,.T.);
#1517=EDGE_CURVE('',#1277,#1276,#163,.T.);
#1518=EDGE_CURVE('',#1278,#1277,#164,.T.);
#1519=EDGE_CURVE('',#1279,#1278,#165,.T.);
#1520=EDGE_CURVE('',#1280,#1279,#166,.T.);
#1521=EDGE_CURVE('',#1281,#1280,#167,.T.);
#1522=EDGE_CURVE('',#1276,#1281,#168,.T.);
#1523=EDGE_CURVE('',#1272,#1281,#835,.T.);
#1524=EDGE_CURVE('',#1273,#1280,#836,.T.);
#1525=EDGE_CURVE('',#1270,#1276,#837,.T.);
#1526=EDGE_CURVE('',#1268,#1277,#838,.T.);
#1527=EDGE_CURVE('',#1282,#1282,#1103,.F.);
#1528=EDGE_CURVE('',#1282,#1283,#839,.T.);
#1529=EDGE_CURVE('',#1283,#1283,#1104,.F.);
#1530=EDGE_CURVE('',#1269,#1278,#840,.T.);
#1531=EDGE_CURVE('',#1274,#1279,#841,.T.);
#1532=EDGE_CURVE('',#1284,#1284,#1105,.T.);
#1533=EDGE_CURVE('',#1284,#1285,#842,.T.);
#1534=EDGE_CURVE('',#1285,#1285,#1106,.T.);
#1535=EDGE_CURVE('',#1286,#1287,#1107,.T.);
#1536=EDGE_CURVE('',#1288,#1286,#843,.T.);
#1537=EDGE_CURVE('',#1289,#1288,#1108,.T.);
#1538=EDGE_CURVE('',#1287,#1289,#844,.T.);
#1539=EDGE_CURVE('',#1290,#1291,#845,.T.);
#1540=EDGE_CURVE('',#1292,#1290,#1109,.T.);
#1541=EDGE_CURVE('',#1293,#1292,#846,.T.);
#1542=EDGE_CURVE('',#1291,#1293,#1110,.T.);
#1543=EDGE_CURVE('',#1290,#1294,#847,.T.);
#1544=EDGE_CURVE('',#1294,#1295,#848,.T.);
#1545=EDGE_CURVE('',#1295,#1296,#849,.T.);
#1546=EDGE_CURVE('',#1296,#1297,#850,.T.);
#1547=EDGE_CURVE('',#1298,#1297,#851,.T.);
#1548=EDGE_CURVE('',#1299,#1298,#852,.T.);
#1549=EDGE_CURVE('',#1299,#1292,#853,.T.);
#1550=EDGE_CURVE('',#1300,#1291,#854,.T.);
#1551=EDGE_CURVE('',#1300,#1294,#855,.T.);
#1552=EDGE_CURVE('',#1301,#1299,#856,.T.);
#1553=EDGE_CURVE('',#1293,#1301,#857,.T.);
#1554=EDGE_CURVE('',#1288,#1302,#858,.T.);
#1555=EDGE_CURVE('',#1302,#1303,#859,.T.);
#1556=EDGE_CURVE('',#1304,#1303,#860,.T.);
#1557=EDGE_CURVE('',#1305,#1304,#861,.T.);
#1558=EDGE_CURVE('',#1305,#1306,#862,.T.);
#1559=EDGE_CURVE('',#1306,#1307,#863,.T.);
#1560=EDGE_CURVE('',#1307,#1289,#864,.T.);
#1561=EDGE_CURVE('',#1308,#1286,#865,.T.);
#1562=EDGE_CURVE('',#1302,#1308,#866,.T.);
#1563=EDGE_CURVE('',#1295,#1309,#867,.T.);
#1564=EDGE_CURVE('',#1309,#1300,#868,.T.);
#1565=EDGE_CURVE('',#1301,#1310,#869,.T.);
#1566=EDGE_CURVE('',#1309,#1310,#870,.T.);
#1567=EDGE_CURVE('',#1311,#1310,#871,.T.);
#1568=EDGE_CURVE('',#1311,#1312,#872,.T.);
#1569=EDGE_CURVE('',#1312,#1306,#873,.T.);
#1570=EDGE_CURVE('',#1296,#1305,#874,.T.);
#1571=EDGE_CURVE('',#1303,#1298,#875,.T.);
#1572=EDGE_CURVE('',#1311,#1308,#876,.T.);
#1573=EDGE_CURVE('',#1287,#1313,#877,.T.);
#1574=EDGE_CURVE('',#1313,#1312,#878,.T.);
#1575=EDGE_CURVE('',#1307,#1313,#879,.T.);
#1576=EDGE_CURVE('',#1297,#1304,#880,.T.);
#1577=EDGE_CURVE('',#1314,#1314,#1111,.T.);
#1578=EDGE_CURVE('',#1314,#1315,#881,.T.);
#1579=EDGE_CURVE('',#1315,#1315,#1112,.T.);
#1580=EDGE_CURVE('',#1316,#1316,#1113,.T.);
#1581=EDGE_CURVE('',#1316,#1317,#882,.T.);
#1582=EDGE_CURVE('',#1317,#1317,#1114,.T.);
#1583=EDGE_CURVE('',#1318,#1318,#1115,.T.);
#1584=EDGE_CURVE('',#1318,#1319,#883,.T.);
#1585=EDGE_CURVE('',#1319,#1319,#1116,.T.);
#1586=EDGE_CURVE('',#1320,#1320,#1117,.T.);
#1587=EDGE_CURVE('',#1320,#1321,#884,.T.);
#1588=EDGE_CURVE('',#1321,#1321,#1118,.T.);
#1589=EDGE_CURVE('',#1322,#1322,#1119,.T.);
#1590=EDGE_CURVE('',#1322,#1323,#885,.T.);
#1591=EDGE_CURVE('',#1323,#1323,#1120,.T.);
#1592=EDGE_CURVE('',#1324,#1324,#1121,.T.);
#1593=EDGE_CURVE('',#1324,#1325,#886,.T.);
#1594=EDGE_CURVE('',#1325,#1325,#1122,.T.);
#1595=EDGE_CURVE('',#1326,#1326,#1123,.T.);
#1596=EDGE_CURVE('',#1326,#1327,#887,.T.);
#1597=EDGE_CURVE('',#1327,#1327,#1124,.T.);
#1598=EDGE_CURVE('',#1328,#1328,#1125,.T.);
#1599=EDGE_CURVE('',#1329,#1329,#1126,.T.);
#1600=EDGE_CURVE('',#1328,#1330,#888,.T.);
#1601=EDGE_CURVE('',#1330,#1330,#1127,.T.);
#1602=EDGE_CURVE('',#1331,#1331,#1128,.T.);
#1603=EDGE_CURVE('',#1331,#1329,#889,.T.);
#1604=EDGE_CURVE('',#1332,#1332,#1129,.T.);
#1605=EDGE_CURVE('',#1332,#1333,#890,.T.);
#1606=EDGE_CURVE('',#1333,#1333,#1130,.T.);
#1607=EDGE_CURVE('',#1334,#1334,#1131,.T.);
#1608=EDGE_CURVE('',#1334,#1335,#891,.T.);
#1609=EDGE_CURVE('',#1335,#1335,#1132,.T.);
#1610=EDGE_CURVE('',#1336,#1336,#1133,.T.);
#1611=EDGE_CURVE('',#1336,#1337,#892,.T.);
#1612=EDGE_CURVE('',#1337,#1337,#1134,.T.);
#1613=EDGE_CURVE('',#1338,#1338,#1135,.T.);
#1614=EDGE_CURVE('',#1338,#1339,#893,.T.);
#1615=EDGE_CURVE('',#1339,#1339,#1136,.T.);
#1616=EDGE_CURVE('',#1340,#1340,#1137,.T.);
#1617=EDGE_CURVE('',#1340,#1341,#894,.T.);
#1618=EDGE_CURVE('',#1341,#1341,#1138,.T.);
#1619=EDGE_CURVE('',#1342,#1342,#1139,.T.);
#1620=EDGE_CURVE('',#1342,#1343,#895,.T.);
#1621=EDGE_CURVE('',#1343,#1343,#1140,.T.);
#1622=EDGE_CURVE('',#1344,#1345,#896,.T.);
#1623=EDGE_CURVE('',#1345,#1346,#897,.T.);
#1624=EDGE_CURVE('',#1346,#1347,#898,.T.);
#1625=EDGE_CURVE('',#1344,#1347,#899,.T.);
#1626=EDGE_CURVE('',#1345,#1348,#900,.T.);
#1627=EDGE_CURVE('',#1348,#1349,#901,.T.);
#1628=EDGE_CURVE('',#1349,#1346,#902,.T.);
#1629=EDGE_CURVE('',#1348,#1350,#903,.T.);
#1630=EDGE_CURVE('',#1350,#1351,#904,.T.);
#1631=EDGE_CURVE('',#1351,#1349,#905,.T.);
#1632=EDGE_CURVE('',#1350,#1352,#906,.T.);
#1633=EDGE_CURVE('',#1352,#1353,#907,.T.);
#1634=EDGE_CURVE('',#1353,#1351,#908,.T.);
#1635=EDGE_CURVE('',#1352,#1354,#909,.T.);
#1636=EDGE_CURVE('',#1354,#1355,#910,.T.);
#1637=EDGE_CURVE('',#1355,#1353,#911,.T.);
#1638=EDGE_CURVE('',#1354,#1344,#912,.T.);
#1639=EDGE_CURVE('',#1347,#1355,#913,.T.);
#1640=EDGE_CURVE('',#1356,#1356,#1141,.T.);
#1641=EDGE_CURVE('',#1357,#1357,#1142,.T.);
#1642=EDGE_CURVE('',#1358,#1358,#1143,.T.);
#1643=EDGE_CURVE('',#1358,#1357,#914,.T.);
#1644=EDGE_CURVE('',#1359,#1359,#1144,.T.);
#1645=EDGE_CURVE('',#1359,#1358,#915,.T.);
#1646=EDGE_CURVE('',#1360,#1360,#1145,.T.);
#1647=EDGE_CURVE('',#1360,#1359,#916,.T.);
#1648=EDGE_CURVE('',#1361,#1361,#1146,.T.);
#1649=EDGE_CURVE('',#1362,#1362,#1147,.F.);
#1650=EDGE_CURVE('',#1362,#1361,#917,.T.);
#1651=EDGE_CURVE('',#1356,#1362,#918,.T.);
#1652=EDGE_CURVE('',#1363,#1363,#1148,.T.);
#1653=EDGE_CURVE('',#1363,#1364,#919,.T.);
#1654=EDGE_CURVE('',#1364,#1364,#1149,.T.);
#1655=EDGE_CURVE('',#1365,#1365,#1150,.T.);
#1656=EDGE_CURVE('',#1366,#1366,#1151,.T.);
#1657=EDGE_CURVE('',#1366,#1367,#920,.T.);
#1658=EDGE_CURVE('',#1367,#1367,#1152,.T.);
#1659=EDGE_CURVE('',#1368,#1368,#1153,.T.);
#1660=EDGE_CURVE('',#1365,#1368,#921,.T.);
#1661=EDGE_CURVE('',#1369,#1369,#1154,.T.);
#1662=EDGE_CURVE('',#1369,#1370,#922,.T.);
#1663=EDGE_CURVE('',#1370,#1370,#1155,.T.);
#1664=EDGE_CURVE('',#1371,#1371,#1156,.T.);
#1665=EDGE_CURVE('',#1371,#1372,#923,.T.);
#1666=EDGE_CURVE('',#1372,#1372,#1157,.T.);
#1667=EDGE_CURVE('',#1373,#1373,#1158,.T.);
#1668=EDGE_CURVE('',#1373,#1374,#924,.T.);
#1669=EDGE_CURVE('',#1374,#1374,#1159,.T.);
#1670=EDGE_CURVE('',#1375,#1375,#1160,.T.);
#1671=EDGE_CURVE('',#1375,#1376,#925,.T.);
#1672=EDGE_CURVE('',#1376,#1376,#1161,.T.);
#1673=EDGE_CURVE('',#1377,#1377,#1162,.T.);
#1674=EDGE_CURVE('',#1377,#1378,#926,.T.);
#1675=EDGE_CURVE('',#1378,#1378,#1163,.T.);
#1676=EDGE_CURVE('',#1379,#1380,#1164,.T.);
#1677=EDGE_CURVE('',#1380,#1379,#1165,.T.);
#1678=EDGE_CURVE('',#1380,#1381,#1166,.T.);
#1679=EDGE_CURVE('',#1382,#1381,#1167,.T.);
#1680=EDGE_CURVE('',#1381,#1382,#1168,.T.);
#1681=EDGE_CURVE('',#1382,#1383,#927,.T.);
#1682=EDGE_CURVE('',#1383,#1383,#1169,.T.);
#1683=EDGE_CURVE('',#1384,#1384,#1170,.T.);
#1684=EDGE_CURVE('',#1384,#1385,#928,.T.);
#1685=EDGE_CURVE('',#1385,#1385,#1171,.T.);
#1686=EDGE_CURVE('',#1385,#1386,#929,.T.);
#1687=EDGE_CURVE('',#1386,#1386,#1172,.T.);
#1688=EDGE_CURVE('',#1387,#1387,#1173,.T.);
#1689=EDGE_CURVE('',#1387,#1379,#930,.T.);
#1690=EDGE_CURVE('',#1388,#1388,#1174,.T.);
#1691=EDGE_CURVE('',#1388,#1384,#931,.T.);
#1692=EDGE_CURVE('',#1389,#1390,#1175,.T.);
#1693=EDGE_CURVE('',#1390,#1389,#1176,.T.);
#1694=EDGE_CURVE('',#1390,#1391,#1177,.T.);
#1695=EDGE_CURVE('',#1392,#1391,#1178,.T.);
#1696=EDGE_CURVE('',#1391,#1392,#1179,.T.);
#1697=EDGE_CURVE('',#1393,#1393,#1180,.T.);
#1698=EDGE_CURVE('',#1393,#1392,#932,.T.);
#1699=EDGE_CURVE('',#1394,#1394,#1181,.T.);
#1700=EDGE_CURVE('',#1395,#1395,#1182,.T.);
#1701=EDGE_CURVE('',#1396,#1396,#1183,.T.);
#1702=EDGE_CURVE('',#1396,#1394,#933,.T.);
#1703=EDGE_CURVE('',#1397,#1397,#1184,.T.);
#1704=EDGE_CURVE('',#1397,#1396,#934,.T.);
#1705=EDGE_CURVE('',#1398,#1398,#1185,.T.);
#1706=EDGE_CURVE('',#1398,#1397,#935,.T.);
#1707=EDGE_CURVE('',#1389,#1395,#936,.T.);
#1708=EDGE_CURVE('',#1399,#1400,#1186,.T.);
#1709=EDGE_CURVE('',#1401,#1402,#1187,.T.);
#1710=EDGE_CURVE('',#1403,#1404,#1188,.T.);
#1711=EDGE_CURVE('',#1405,#1406,#1189,.T.);
#1712=EDGE_CURVE('',#1407,#1408,#1190,.T.);
#1713=EDGE_CURVE('',#1409,#1410,#1191,.T.);
#1714=EDGE_CURVE('',#1411,#1412,#1192,.T.);
#1715=EDGE_CURVE('',#1413,#1414,#1193,.T.);
#1716=EDGE_CURVE('',#1415,#1416,#11,.T.);
#1717=EDGE_CURVE('',#1417,#1415,#1194,.T.);
#1718=EDGE_CURVE('',#1418,#1417,#12,.T.);
#1719=EDGE_CURVE('',#1416,#1418,#1195,.T.);
#1720=EDGE_CURVE('',#1419,#1417,#1196,.T.);
#1721=EDGE_CURVE('',#1419,#1420,#13,.T.);
#1722=EDGE_CURVE('',#1421,#1420,#1197,.T.);
#1723=EDGE_CURVE('',#1421,#1422,#14,.T.);
#1724=EDGE_CURVE('',#1423,#1422,#1198,.T.);
#1725=EDGE_CURVE('',#1423,#1424,#15,.T.);
#1726=EDGE_CURVE('',#1424,#1425,#937,.T.);
#1727=EDGE_CURVE('',#1425,#1425,#1199,.T.);
#1728=EDGE_CURVE('',#1424,#1426,#16,.T.);
#1729=EDGE_CURVE('',#1427,#1426,#1200,.T.);
#1730=EDGE_CURVE('',#1427,#1428,#17,.T.);
#1731=EDGE_CURVE('',#1429,#1428,#1201,.T.);
#1732=EDGE_CURVE('',#1429,#1430,#18,.T.);
#1733=EDGE_CURVE('',#1431,#1430,#1202,.T.);
#1734=EDGE_CURVE('',#1431,#1432,#19,.T.);
#1735=EDGE_CURVE('',#1433,#1432,#1203,.T.);
#1736=EDGE_CURVE('',#1433,#1434,#20,.T.);
#1737=EDGE_CURVE('',#1418,#1434,#1204,.T.);
#1738=EDGE_CURVE('',#1415,#1435,#1205,.T.);
#1739=EDGE_CURVE('',#1435,#1419,#1206,.T.);
#1740=EDGE_CURVE('',#1436,#1435,#21,.T.);
#1741=EDGE_CURVE('',#1420,#1436,#1207,.T.);
#1742=EDGE_CURVE('',#1436,#1437,#1208,.T.);
#1743=EDGE_CURVE('',#1437,#1421,#1209,.T.);
#1744=EDGE_CURVE('',#1438,#1437,#22,.T.);
#1745=EDGE_CURVE('',#1422,#1438,#1210,.T.);
#1746=EDGE_CURVE('',#1438,#1439,#1211,.T.);
#1747=EDGE_CURVE('',#1439,#1423,#1212,.T.);
#1748=EDGE_CURVE('',#1440,#1441,#23,.T.);
#1749=EDGE_CURVE('',#1426,#1440,#1213,.T.);
#1750=EDGE_CURVE('',#1441,#1439,#24,.T.);
#1751=EDGE_CURVE('',#1440,#1442,#1214,.T.);
#1752=EDGE_CURVE('',#1442,#1427,#1215,.T.);
#1753=EDGE_CURVE('',#1443,#1442,#25,.T.);
#1754=EDGE_CURVE('',#1428,#1443,#1216,.T.);
#1755=EDGE_CURVE('',#1443,#1444,#1217,.T.);
#1756=EDGE_CURVE('',#1444,#1429,#1218,.T.);
#1757=EDGE_CURVE('',#1445,#1444,#26,.T.);
#1758=EDGE_CURVE('',#1430,#1445,#1219,.T.);
#1759=EDGE_CURVE('',#1445,#1446,#1220,.T.);
#1760=EDGE_CURVE('',#1446,#1431,#1221,.T.);
#1761=EDGE_CURVE('',#1447,#1446,#27,.T.);
#1762=EDGE_CURVE('',#1432,#1447,#1222,.T.);
#1763=EDGE_CURVE('',#1448,#1448,#1223,.T.);
#1764=EDGE_CURVE('',#1448,#1441,#938,.T.);
#1765=EDGE_CURVE('',#1449,#1416,#1224,.T.);
#1766=EDGE_CURVE('',#1449,#1450,#28,.T.);
#1767=EDGE_CURVE('',#1447,#1450,#1225,.T.);
#1768=EDGE_CURVE('',#1434,#1449,#1226,.T.);
#1769=EDGE_CURVE('',#1450,#1433,#1227,.T.);
#1770=EDGE_CURVE('',#1451,#1451,#1228,.T.);
#1771=EDGE_CURVE('',#1452,#1452,#1229,.T.);
#1772=EDGE_CURVE('',#1453,#1453,#1230,.T.);
#1773=EDGE_CURVE('',#1453,#1451,#939,.T.);
#1774=EDGE_CURVE('',#1454,#1454,#1231,.T.);
#1775=EDGE_CURVE('',#1454,#1452,#940,.T.);
#1776=EDGE_CURVE('',#1455,#1455,#1232,.T.);
#1777=EDGE_CURVE('',#1456,#1456,#1233,.T.);
#1778=EDGE_CURVE('',#1457,#1457,#1234,.T.);
#1779=EDGE_CURVE('',#1457,#1455,#941,.T.);
#1780=EDGE_CURVE('',#1458,#1458,#1235,.T.);
#1781=EDGE_CURVE('',#1458,#1456,#942,.T.);
#1782=ORIENTED_EDGE('',*,*,#1459,.F.);
#1783=ORIENTED_EDGE('',*,*,#1460,.T.);
#1784=ORIENTED_EDGE('',*,*,#1461,.F.);
#1785=ORIENTED_EDGE('',*,*,#1460,.F.);
#1786=ORIENTED_EDGE('',*,*,#1462,.F.);
#1787=ORIENTED_EDGE('',*,*,#1463,.T.);
#1788=ORIENTED_EDGE('',*,*,#1464,.F.);
#1789=ORIENTED_EDGE('',*,*,#1463,.F.);
#1790=ORIENTED_EDGE('',*,*,#1465,.F.);
#1791=ORIENTED_EDGE('',*,*,#1466,.T.);
#1792=ORIENTED_EDGE('',*,*,#1467,.F.);
#1793=ORIENTED_EDGE('',*,*,#1466,.F.);
#1794=ORIENTED_EDGE('',*,*,#1468,.F.);
#1795=ORIENTED_EDGE('',*,*,#1469,.T.);
#1796=ORIENTED_EDGE('',*,*,#1470,.F.);
#1797=ORIENTED_EDGE('',*,*,#1469,.F.);
#1798=ORIENTED_EDGE('',*,*,#1471,.F.);
#1799=ORIENTED_EDGE('',*,*,#1472,.T.);
#1800=ORIENTED_EDGE('',*,*,#1473,.F.);
#1801=ORIENTED_EDGE('',*,*,#1472,.F.);
#1802=ORIENTED_EDGE('',*,*,#1474,.T.);
#1803=ORIENTED_EDGE('',*,*,#1475,.T.);
#1804=ORIENTED_EDGE('',*,*,#1476,.F.);
#1805=ORIENTED_EDGE('',*,*,#1477,.F.);
#1806=ORIENTED_EDGE('',*,*,#1478,.T.);
#1807=ORIENTED_EDGE('',*,*,#1477,.T.);
#1808=ORIENTED_EDGE('',*,*,#1479,.F.);
#1809=ORIENTED_EDGE('',*,*,#1480,.F.);
#1810=ORIENTED_EDGE('',*,*,#1481,.T.);
#1811=ORIENTED_EDGE('',*,*,#1480,.T.);
#1812=ORIENTED_EDGE('',*,*,#1482,.F.);
#1813=ORIENTED_EDGE('',*,*,#1483,.F.);
#1814=ORIENTED_EDGE('',*,*,#1484,.T.);
#1815=ORIENTED_EDGE('',*,*,#1483,.T.);
#1816=ORIENTED_EDGE('',*,*,#1485,.F.);
#1817=ORIENTED_EDGE('',*,*,#1475,.F.);
#1818=ORIENTED_EDGE('',*,*,#1485,.T.);
#1819=ORIENTED_EDGE('',*,*,#1482,.T.);
#1820=ORIENTED_EDGE('',*,*,#1479,.T.);
#1821=ORIENTED_EDGE('',*,*,#1476,.T.);
#1822=ORIENTED_EDGE('',*,*,#1461,.T.);
#1823=ORIENTED_EDGE('',*,*,#1464,.T.);
#1824=ORIENTED_EDGE('',*,*,#1467,.T.);
#1825=ORIENTED_EDGE('',*,*,#1470,.T.);
#1826=ORIENTED_EDGE('',*,*,#1473,.T.);
#1827=ORIENTED_EDGE('',*,*,#1484,.F.);
#1828=ORIENTED_EDGE('',*,*,#1474,.F.);
#1829=ORIENTED_EDGE('',*,*,#1478,.F.);
#1830=ORIENTED_EDGE('',*,*,#1481,.F.);
#1831=ORIENTED_EDGE('',*,*,#1459,.T.);
#1832=ORIENTED_EDGE('',*,*,#1462,.T.);
#1833=ORIENTED_EDGE('',*,*,#1465,.T.);
#1834=ORIENTED_EDGE('',*,*,#1468,.T.);
#1835=ORIENTED_EDGE('',*,*,#1471,.T.);
#1836=ORIENTED_EDGE('',*,*,#1486,.F.);
#1837=ORIENTED_EDGE('',*,*,#1487,.T.);
#1838=ORIENTED_EDGE('',*,*,#1488,.T.);
#1839=ORIENTED_EDGE('',*,*,#1487,.F.);
#1840=ORIENTED_EDGE('',*,*,#1488,.F.);
#1841=ORIENTED_EDGE('',*,*,#1489,.F.);
#1842=ORIENTED_EDGE('',*,*,#1490,.T.);
#1843=ORIENTED_EDGE('',*,*,#1491,.F.);
#1844=ORIENTED_EDGE('',*,*,#1492,.T.);
#1845=ORIENTED_EDGE('',*,*,#1489,.T.);
#1846=ORIENTED_EDGE('',*,*,#1492,.F.);
#1847=ORIENTED_EDGE('',*,*,#1491,.T.);
#1848=ORIENTED_EDGE('',*,*,#1490,.F.);
#1849=ORIENTED_EDGE('',*,*,#1493,.T.);
#1850=ORIENTED_EDGE('',*,*,#1494,.T.);
#1851=ORIENTED_EDGE('',*,*,#1493,.F.);
#1852=ORIENTED_EDGE('',*,*,#1494,.F.);
#1853=ORIENTED_EDGE('',*,*,#1486,.T.);
#1854=ORIENTED_EDGE('',*,*,#1495,.F.);
#1855=ORIENTED_EDGE('',*,*,#1496,.T.);
#1856=ORIENTED_EDGE('',*,*,#1497,.T.);
#1857=ORIENTED_EDGE('',*,*,#1496,.F.);
#1858=ORIENTED_EDGE('',*,*,#1498,.F.);
#1859=ORIENTED_EDGE('',*,*,#1499,.T.);
#1860=ORIENTED_EDGE('',*,*,#1500,.T.);
#1861=ORIENTED_EDGE('',*,*,#1499,.F.);
#1862=ORIENTED_EDGE('',*,*,#1498,.T.);
#1863=ORIENTED_EDGE('',*,*,#1495,.T.);
#1864=ORIENTED_EDGE('',*,*,#1500,.F.);
#1865=ORIENTED_EDGE('',*,*,#1497,.F.);
#1866=ORIENTED_EDGE('',*,*,#1501,.F.);
#1867=ORIENTED_EDGE('',*,*,#1502,.T.);
#1868=ORIENTED_EDGE('',*,*,#1503,.T.);
#1869=ORIENTED_EDGE('',*,*,#1502,.F.);
#1870=ORIENTED_EDGE('',*,*,#1504,.F.);
#1871=ORIENTED_EDGE('',*,*,#1505,.T.);
#1872=ORIENTED_EDGE('',*,*,#1506,.T.);
#1873=ORIENTED_EDGE('',*,*,#1505,.F.);
#1874=ORIENTED_EDGE('',*,*,#1504,.T.);
#1875=ORIENTED_EDGE('',*,*,#1501,.T.);
#1876=ORIENTED_EDGE('',*,*,#1506,.F.);
#1877=ORIENTED_EDGE('',*,*,#1503,.F.);
#1878=ORIENTED_EDGE('',*,*,#1507,.F.);
#1879=ORIENTED_EDGE('',*,*,#1508,.F.);
#1880=ORIENTED_EDGE('',*,*,#1509,.T.);
#1881=ORIENTED_EDGE('',*,*,#1510,.F.);
#1882=ORIENTED_EDGE('',*,*,#1509,.F.);
#1883=ORIENTED_EDGE('',*,*,#1511,.F.);
#1884=ORIENTED_EDGE('',*,*,#1512,.F.);
#1885=ORIENTED_EDGE('',*,*,#1513,.F.);
#1886=ORIENTED_EDGE('',*,*,#1514,.F.);
#1887=ORIENTED_EDGE('',*,*,#1515,.F.);
#1888=ORIENTED_EDGE('',*,*,#1516,.T.);
#1889=ORIENTED_EDGE('',*,*,#1517,.F.);
#1890=ORIENTED_EDGE('',*,*,#1518,.F.);
#1891=ORIENTED_EDGE('',*,*,#1519,.F.);
#1892=ORIENTED_EDGE('',*,*,#1520,.F.);
#1893=ORIENTED_EDGE('',*,*,#1521,.F.);
#1894=ORIENTED_EDGE('',*,*,#1522,.F.);
#1895=ORIENTED_EDGE('',*,*,#1516,.F.);
#1896=ORIENTED_EDGE('',*,*,#1512,.T.);
#1897=ORIENTED_EDGE('',*,*,#1523,.T.);
#1898=ORIENTED_EDGE('',*,*,#1521,.T.);
#1899=ORIENTED_EDGE('',*,*,#1524,.F.);
#1900=ORIENTED_EDGE('',*,*,#1511,.T.);
#1901=ORIENTED_EDGE('',*,*,#1525,.T.);
#1902=ORIENTED_EDGE('',*,*,#1522,.T.);
#1903=ORIENTED_EDGE('',*,*,#1523,.F.);
#1904=ORIENTED_EDGE('',*,*,#1508,.T.);
#1905=ORIENTED_EDGE('',*,*,#1526,.T.);
#1906=ORIENTED_EDGE('',*,*,#1517,.T.);
#1907=ORIENTED_EDGE('',*,*,#1525,.F.);
#1908=ORIENTED_EDGE('',*,*,#1527,.F.);
#1909=ORIENTED_EDGE('',*,*,#1528,.T.);
#1910=ORIENTED_EDGE('',*,*,#1529,.T.);
#1911=ORIENTED_EDGE('',*,*,#1528,.F.);
#1912=ORIENTED_EDGE('',*,*,#1507,.T.);
#1913=ORIENTED_EDGE('',*,*,#1530,.T.);
#1914=ORIENTED_EDGE('',*,*,#1518,.T.);
#1915=ORIENTED_EDGE('',*,*,#1526,.F.);
#1916=ORIENTED_EDGE('',*,*,#1513,.T.);
#1917=ORIENTED_EDGE('',*,*,#1524,.T.);
#1918=ORIENTED_EDGE('',*,*,#1520,.T.);
#1919=ORIENTED_EDGE('',*,*,#1531,.F.);
#1920=ORIENTED_EDGE('',*,*,#1514,.T.);
#1921=ORIENTED_EDGE('',*,*,#1531,.T.);
#1922=ORIENTED_EDGE('',*,*,#1519,.T.);
#1923=ORIENTED_EDGE('',*,*,#1530,.F.);
#1924=ORIENTED_EDGE('',*,*,#1515,.T.);
#1925=ORIENTED_EDGE('',*,*,#1527,.T.);
#1926=ORIENTED_EDGE('',*,*,#1510,.T.);
#1927=ORIENTED_EDGE('',*,*,#1529,.F.);
#1928=ORIENTED_EDGE('',*,*,#1532,.F.);
#1929=ORIENTED_EDGE('',*,*,#1533,.T.);
#1930=ORIENTED_EDGE('',*,*,#1534,.F.);
#1931=ORIENTED_EDGE('',*,*,#1533,.F.);
#1932=ORIENTED_EDGE('',*,*,#1535,.F.);
#1933=ORIENTED_EDGE('',*,*,#1536,.F.);
#1934=ORIENTED_EDGE('',*,*,#1537,.F.);
#1935=ORIENTED_EDGE('',*,*,#1538,.F.);
#1936=ORIENTED_EDGE('',*,*,#1539,.F.);
#1937=ORIENTED_EDGE('',*,*,#1540,.F.);
#1938=ORIENTED_EDGE('',*,*,#1541,.F.);
#1939=ORIENTED_EDGE('',*,*,#1542,.F.);
#1940=ORIENTED_EDGE('',*,*,#1540,.T.);
#1941=ORIENTED_EDGE('',*,*,#1543,.T.);
#1942=ORIENTED_EDGE('',*,*,#1544,.T.);
#1943=ORIENTED_EDGE('',*,*,#1545,.T.);
#1944=ORIENTED_EDGE('',*,*,#1546,.T.);
#1945=ORIENTED_EDGE('',*,*,#1547,.F.);
#1946=ORIENTED_EDGE('',*,*,#1548,.F.);
#1947=ORIENTED_EDGE('',*,*,#1549,.T.);
#1948=ORIENTED_EDGE('',*,*,#1539,.T.);
#1949=ORIENTED_EDGE('',*,*,#1550,.F.);
#1950=ORIENTED_EDGE('',*,*,#1551,.T.);
#1951=ORIENTED_EDGE('',*,*,#1543,.F.);
#1952=ORIENTED_EDGE('',*,*,#1541,.T.);
#1953=ORIENTED_EDGE('',*,*,#1549,.F.);
#1954=ORIENTED_EDGE('',*,*,#1552,.F.);
#1955=ORIENTED_EDGE('',*,*,#1553,.F.);
#1956=ORIENTED_EDGE('',*,*,#1537,.T.);
#1957=ORIENTED_EDGE('',*,*,#1554,.T.);
#1958=ORIENTED_EDGE('',*,*,#1555,.T.);
#1959=ORIENTED_EDGE('',*,*,#1556,.F.);
#1960=ORIENTED_EDGE('',*,*,#1557,.F.);
#1961=ORIENTED_EDGE('',*,*,#1558,.T.);
#1962=ORIENTED_EDGE('',*,*,#1559,.T.);
#1963=ORIENTED_EDGE('',*,*,#1560,.T.);
#1964=ORIENTED_EDGE('',*,*,#1536,.T.);
#1965=ORIENTED_EDGE('',*,*,#1561,.F.);
#1966=ORIENTED_EDGE('',*,*,#1562,.F.);
#1967=ORIENTED_EDGE('',*,*,#1554,.F.);
#1968=ORIENTED_EDGE('',*,*,#1563,.F.);
#1969=ORIENTED_EDGE('',*,*,#1544,.F.);
#1970=ORIENTED_EDGE('',*,*,#1551,.F.);
#1971=ORIENTED_EDGE('',*,*,#1564,.F.);
#1972=ORIENTED_EDGE('',*,*,#1542,.T.);
#1973=ORIENTED_EDGE('',*,*,#1553,.T.);
#1974=ORIENTED_EDGE('',*,*,#1565,.T.);
#1975=ORIENTED_EDGE('',*,*,#1566,.F.);
#1976=ORIENTED_EDGE('',*,*,#1564,.T.);
#1977=ORIENTED_EDGE('',*,*,#1550,.T.);
#1978=ORIENTED_EDGE('',*,*,#1563,.T.);
#1979=ORIENTED_EDGE('',*,*,#1566,.T.);
#1980=ORIENTED_EDGE('',*,*,#1567,.F.);
#1981=ORIENTED_EDGE('',*,*,#1568,.T.);
#1982=ORIENTED_EDGE('',*,*,#1569,.T.);
#1983=ORIENTED_EDGE('',*,*,#1558,.F.);
#1984=ORIENTED_EDGE('',*,*,#1570,.F.);
#1985=ORIENTED_EDGE('',*,*,#1545,.F.);
#1986=ORIENTED_EDGE('',*,*,#1532,.T.);
#1987=ORIENTED_EDGE('',*,*,#1548,.T.);
#1988=ORIENTED_EDGE('',*,*,#1571,.F.);
#1989=ORIENTED_EDGE('',*,*,#1555,.F.);
#1990=ORIENTED_EDGE('',*,*,#1562,.T.);
#1991=ORIENTED_EDGE('',*,*,#1572,.F.);
#1992=ORIENTED_EDGE('',*,*,#1567,.T.);
#1993=ORIENTED_EDGE('',*,*,#1565,.F.);
#1994=ORIENTED_EDGE('',*,*,#1552,.T.);
#1995=ORIENTED_EDGE('',*,*,#1535,.T.);
#1996=ORIENTED_EDGE('',*,*,#1573,.T.);
#1997=ORIENTED_EDGE('',*,*,#1574,.T.);
#1998=ORIENTED_EDGE('',*,*,#1568,.F.);
#1999=ORIENTED_EDGE('',*,*,#1572,.T.);
#2000=ORIENTED_EDGE('',*,*,#1561,.T.);
#2001=ORIENTED_EDGE('',*,*,#1569,.F.);
#2002=ORIENTED_EDGE('',*,*,#1574,.F.);
#2003=ORIENTED_EDGE('',*,*,#1575,.F.);
#2004=ORIENTED_EDGE('',*,*,#1559,.F.);
#2005=ORIENTED_EDGE('',*,*,#1538,.T.);
#2006=ORIENTED_EDGE('',*,*,#1560,.F.);
#2007=ORIENTED_EDGE('',*,*,#1575,.T.);
#2008=ORIENTED_EDGE('',*,*,#1573,.F.);
#2009=ORIENTED_EDGE('',*,*,#1570,.T.);
#2010=ORIENTED_EDGE('',*,*,#1557,.T.);
#2011=ORIENTED_EDGE('',*,*,#1576,.F.);
#2012=ORIENTED_EDGE('',*,*,#1546,.F.);
#2013=ORIENTED_EDGE('',*,*,#1576,.T.);
#2014=ORIENTED_EDGE('',*,*,#1556,.T.);
#2015=ORIENTED_EDGE('',*,*,#1571,.T.);
#2016=ORIENTED_EDGE('',*,*,#1547,.T.);
#2017=ORIENTED_EDGE('',*,*,#1534,.T.);
#2018=ORIENTED_EDGE('',*,*,#1577,.F.);
#2019=ORIENTED_EDGE('',*,*,#1578,.T.);
#2020=ORIENTED_EDGE('',*,*,#1579,.T.);
#2021=ORIENTED_EDGE('',*,*,#1578,.F.);
#2022=ORIENTED_EDGE('',*,*,#1580,.F.);
#2023=ORIENTED_EDGE('',*,*,#1581,.T.);
#2024=ORIENTED_EDGE('',*,*,#1582,.T.);
#2025=ORIENTED_EDGE('',*,*,#1581,.F.);
#2026=ORIENTED_EDGE('',*,*,#1580,.T.);
#2027=ORIENTED_EDGE('',*,*,#1577,.T.);
#2028=ORIENTED_EDGE('',*,*,#1582,.F.);
#2029=ORIENTED_EDGE('',*,*,#1579,.F.);
#2030=ORIENTED_EDGE('',*,*,#1583,.F.);
#2031=ORIENTED_EDGE('',*,*,#1584,.T.);
#2032=ORIENTED_EDGE('',*,*,#1585,.T.);
#2033=ORIENTED_EDGE('',*,*,#1584,.F.);
#2034=ORIENTED_EDGE('',*,*,#1586,.F.);
#2035=ORIENTED_EDGE('',*,*,#1587,.T.);
#2036=ORIENTED_EDGE('',*,*,#1588,.T.);
#2037=ORIENTED_EDGE('',*,*,#1587,.F.);
#2038=ORIENTED_EDGE('',*,*,#1586,.T.);
#2039=ORIENTED_EDGE('',*,*,#1583,.T.);
#2040=ORIENTED_EDGE('',*,*,#1588,.F.);
#2041=ORIENTED_EDGE('',*,*,#1585,.F.);
#2042=ORIENTED_EDGE('',*,*,#1589,.F.);
#2043=ORIENTED_EDGE('',*,*,#1590,.T.);
#2044=ORIENTED_EDGE('',*,*,#1591,.T.);
#2045=ORIENTED_EDGE('',*,*,#1590,.F.);
#2046=ORIENTED_EDGE('',*,*,#1592,.F.);
#2047=ORIENTED_EDGE('',*,*,#1593,.T.);
#2048=ORIENTED_EDGE('',*,*,#1594,.T.);
#2049=ORIENTED_EDGE('',*,*,#1593,.F.);
#2050=ORIENTED_EDGE('',*,*,#1592,.T.);
#2051=ORIENTED_EDGE('',*,*,#1589,.T.);
#2052=ORIENTED_EDGE('',*,*,#1594,.F.);
#2053=ORIENTED_EDGE('',*,*,#1591,.F.);
#2054=ORIENTED_EDGE('',*,*,#1595,.F.);
#2055=ORIENTED_EDGE('',*,*,#1596,.T.);
#2056=ORIENTED_EDGE('',*,*,#1597,.F.);
#2057=ORIENTED_EDGE('',*,*,#1596,.F.);
#2058=ORIENTED_EDGE('',*,*,#1595,.T.);
#2059=ORIENTED_EDGE('',*,*,#1598,.T.);
#2060=ORIENTED_EDGE('',*,*,#1599,.F.);
#2061=ORIENTED_EDGE('',*,*,#1598,.F.);
#2062=ORIENTED_EDGE('',*,*,#1600,.T.);
#2063=ORIENTED_EDGE('',*,*,#1601,.T.);
#2064=ORIENTED_EDGE('',*,*,#1600,.F.);
#2065=ORIENTED_EDGE('',*,*,#1601,.F.);
#2066=ORIENTED_EDGE('',*,*,#1602,.F.);
#2067=ORIENTED_EDGE('',*,*,#1603,.T.);
#2068=ORIENTED_EDGE('',*,*,#1599,.T.);
#2069=ORIENTED_EDGE('',*,*,#1603,.F.);
#2070=ORIENTED_EDGE('',*,*,#1602,.T.);
#2071=ORIENTED_EDGE('',*,*,#1597,.T.);
#2072=ORIENTED_EDGE('',*,*,#1604,.F.);
#2073=ORIENTED_EDGE('',*,*,#1605,.T.);
#2074=ORIENTED_EDGE('',*,*,#1606,.T.);
#2075=ORIENTED_EDGE('',*,*,#1605,.F.);
#2076=ORIENTED_EDGE('',*,*,#1607,.F.);
#2077=ORIENTED_EDGE('',*,*,#1608,.T.);
#2078=ORIENTED_EDGE('',*,*,#1609,.T.);
#2079=ORIENTED_EDGE('',*,*,#1608,.F.);
#2080=ORIENTED_EDGE('',*,*,#1607,.T.);
#2081=ORIENTED_EDGE('',*,*,#1604,.T.);
#2082=ORIENTED_EDGE('',*,*,#1609,.F.);
#2083=ORIENTED_EDGE('',*,*,#1606,.F.);
#2084=ORIENTED_EDGE('',*,*,#1610,.F.);
#2085=ORIENTED_EDGE('',*,*,#1611,.T.);
#2086=ORIENTED_EDGE('',*,*,#1612,.T.);
#2087=ORIENTED_EDGE('',*,*,#1611,.F.);
#2088=ORIENTED_EDGE('',*,*,#1613,.F.);
#2089=ORIENTED_EDGE('',*,*,#1614,.T.);
#2090=ORIENTED_EDGE('',*,*,#1615,.T.);
#2091=ORIENTED_EDGE('',*,*,#1614,.F.);
#2092=ORIENTED_EDGE('',*,*,#1613,.T.);
#2093=ORIENTED_EDGE('',*,*,#1610,.T.);
#2094=ORIENTED_EDGE('',*,*,#1615,.F.);
#2095=ORIENTED_EDGE('',*,*,#1612,.F.);
#2096=ORIENTED_EDGE('',*,*,#1616,.F.);
#2097=ORIENTED_EDGE('',*,*,#1617,.T.);
#2098=ORIENTED_EDGE('',*,*,#1618,.T.);
#2099=ORIENTED_EDGE('',*,*,#1617,.F.);
#2100=ORIENTED_EDGE('',*,*,#1619,.F.);
#2101=ORIENTED_EDGE('',*,*,#1620,.T.);
#2102=ORIENTED_EDGE('',*,*,#1621,.T.);
#2103=ORIENTED_EDGE('',*,*,#1620,.F.);
#2104=ORIENTED_EDGE('',*,*,#1619,.T.);
#2105=ORIENTED_EDGE('',*,*,#1616,.T.);
#2106=ORIENTED_EDGE('',*,*,#1621,.F.);
#2107=ORIENTED_EDGE('',*,*,#1618,.F.);
#2108=ORIENTED_EDGE('',*,*,#1622,.T.);
#2109=ORIENTED_EDGE('',*,*,#1623,.T.);
#2110=ORIENTED_EDGE('',*,*,#1624,.T.);
#2111=ORIENTED_EDGE('',*,*,#1625,.F.);
#2112=ORIENTED_EDGE('',*,*,#1626,.T.);
#2113=ORIENTED_EDGE('',*,*,#1627,.T.);
#2114=ORIENTED_EDGE('',*,*,#1628,.T.);
#2115=ORIENTED_EDGE('',*,*,#1623,.F.);
#2116=ORIENTED_EDGE('',*,*,#1629,.T.);
#2117=ORIENTED_EDGE('',*,*,#1630,.T.);
#2118=ORIENTED_EDGE('',*,*,#1631,.T.);
#2119=ORIENTED_EDGE('',*,*,#1627,.F.);
#2120=ORIENTED_EDGE('',*,*,#1632,.T.);
#2121=ORIENTED_EDGE('',*,*,#1633,.T.);
#2122=ORIENTED_EDGE('',*,*,#1634,.T.);
#2123=ORIENTED_EDGE('',*,*,#1630,.F.);
#2124=ORIENTED_EDGE('',*,*,#1635,.T.);
#2125=ORIENTED_EDGE('',*,*,#1636,.T.);
#2126=ORIENTED_EDGE('',*,*,#1637,.T.);
#2127=ORIENTED_EDGE('',*,*,#1633,.F.);
#2128=ORIENTED_EDGE('',*,*,#1638,.T.);
#2129=ORIENTED_EDGE('',*,*,#1625,.T.);
#2130=ORIENTED_EDGE('',*,*,#1639,.T.);
#2131=ORIENTED_EDGE('',*,*,#1636,.F.);
#2132=ORIENTED_EDGE('',*,*,#1638,.F.);
#2133=ORIENTED_EDGE('',*,*,#1635,.F.);
#2134=ORIENTED_EDGE('',*,*,#1632,.F.);
#2135=ORIENTED_EDGE('',*,*,#1629,.F.);
#2136=ORIENTED_EDGE('',*,*,#1626,.F.);
#2137=ORIENTED_EDGE('',*,*,#1622,.F.);
#2138=ORIENTED_EDGE('',*,*,#1639,.F.);
#2139=ORIENTED_EDGE('',*,*,#1624,.F.);
#2140=ORIENTED_EDGE('',*,*,#1628,.F.);
#2141=ORIENTED_EDGE('',*,*,#1631,.F.);
#2142=ORIENTED_EDGE('',*,*,#1634,.F.);
#2143=ORIENTED_EDGE('',*,*,#1637,.F.);
#2144=ORIENTED_EDGE('',*,*,#1640,.F.);
#2145=ORIENTED_EDGE('',*,*,#1641,.F.);
#2146=ORIENTED_EDGE('',*,*,#1642,.F.);
#2147=ORIENTED_EDGE('',*,*,#1643,.T.);
#2148=ORIENTED_EDGE('',*,*,#1641,.T.);
#2149=ORIENTED_EDGE('',*,*,#1643,.F.);
#2150=ORIENTED_EDGE('',*,*,#1644,.F.);
#2151=ORIENTED_EDGE('',*,*,#1645,.T.);
#2152=ORIENTED_EDGE('',*,*,#1642,.T.);
#2153=ORIENTED_EDGE('',*,*,#1645,.F.);
#2154=ORIENTED_EDGE('',*,*,#1646,.F.);
#2155=ORIENTED_EDGE('',*,*,#1647,.T.);
#2156=ORIENTED_EDGE('',*,*,#1644,.T.);
#2157=ORIENTED_EDGE('',*,*,#1647,.F.);
#2158=ORIENTED_EDGE('',*,*,#1646,.T.);
#2159=ORIENTED_EDGE('',*,*,#1648,.F.);
#2160=ORIENTED_EDGE('',*,*,#1649,.F.);
#2161=ORIENTED_EDGE('',*,*,#1650,.T.);
#2162=ORIENTED_EDGE('',*,*,#1648,.T.);
#2163=ORIENTED_EDGE('',*,*,#1650,.F.);
#2164=ORIENTED_EDGE('',*,*,#1640,.T.);
#2165=ORIENTED_EDGE('',*,*,#1651,.T.);
#2166=ORIENTED_EDGE('',*,*,#1649,.T.);
#2167=ORIENTED_EDGE('',*,*,#1651,.F.);
#2168=ORIENTED_EDGE('',*,*,#1652,.F.);
#2169=ORIENTED_EDGE('',*,*,#1653,.T.);
#2170=ORIENTED_EDGE('',*,*,#1654,.F.);
#2171=ORIENTED_EDGE('',*,*,#1653,.F.);
#2172=ORIENTED_EDGE('',*,*,#1652,.T.);
#2173=ORIENTED_EDGE('',*,*,#1655,.F.);
#2174=ORIENTED_EDGE('',*,*,#1656,.F.);
#2175=ORIENTED_EDGE('',*,*,#1657,.T.);
#2176=ORIENTED_EDGE('',*,*,#1658,.T.);
#2177=ORIENTED_EDGE('',*,*,#1657,.F.);
#2178=ORIENTED_EDGE('',*,*,#1658,.F.);
#2179=ORIENTED_EDGE('',*,*,#1659,.F.);
#2180=ORIENTED_EDGE('',*,*,#1655,.T.);
#2181=ORIENTED_EDGE('',*,*,#1660,.T.);
#2182=ORIENTED_EDGE('',*,*,#1659,.T.);
#2183=ORIENTED_EDGE('',*,*,#1660,.F.);
#2184=ORIENTED_EDGE('',*,*,#1661,.F.);
#2185=ORIENTED_EDGE('',*,*,#1662,.T.);
#2186=ORIENTED_EDGE('',*,*,#1663,.T.);
#2187=ORIENTED_EDGE('',*,*,#1662,.F.);
#2188=ORIENTED_EDGE('',*,*,#1661,.T.);
#2189=ORIENTED_EDGE('',*,*,#1654,.T.);
#2190=ORIENTED_EDGE('',*,*,#1663,.F.);
#2191=ORIENTED_EDGE('',*,*,#1656,.T.);
#2192=ORIENTED_EDGE('',*,*,#1664,.F.);
#2193=ORIENTED_EDGE('',*,*,#1665,.T.);
#2194=ORIENTED_EDGE('',*,*,#1666,.T.);
#2195=ORIENTED_EDGE('',*,*,#1665,.F.);
#2196=ORIENTED_EDGE('',*,*,#1667,.F.);
#2197=ORIENTED_EDGE('',*,*,#1668,.T.);
#2198=ORIENTED_EDGE('',*,*,#1669,.T.);
#2199=ORIENTED_EDGE('',*,*,#1668,.F.);
#2200=ORIENTED_EDGE('',*,*,#1667,.T.);
#2201=ORIENTED_EDGE('',*,*,#1664,.T.);
#2202=ORIENTED_EDGE('',*,*,#1669,.F.);
#2203=ORIENTED_EDGE('',*,*,#1666,.F.);
#2204=ORIENTED_EDGE('',*,*,#1670,.F.);
#2205=ORIENTED_EDGE('',*,*,#1671,.T.);
#2206=ORIENTED_EDGE('',*,*,#1672,.T.);
#2207=ORIENTED_EDGE('',*,*,#1671,.F.);
#2208=ORIENTED_EDGE('',*,*,#1673,.F.);
#2209=ORIENTED_EDGE('',*,*,#1674,.T.);
#2210=ORIENTED_EDGE('',*,*,#1675,.T.);
#2211=ORIENTED_EDGE('',*,*,#1674,.F.);
#2212=ORIENTED_EDGE('',*,*,#1673,.T.);
#2213=ORIENTED_EDGE('',*,*,#1670,.T.);
#2214=ORIENTED_EDGE('',*,*,#1675,.F.);
#2215=ORIENTED_EDGE('',*,*,#1672,.F.);
#2216=ORIENTED_EDGE('',*,*,#1676,.F.);
#2217=ORIENTED_EDGE('',*,*,#1677,.F.);
#2218=ORIENTED_EDGE('',*,*,#1678,.T.);
#2219=ORIENTED_EDGE('',*,*,#1679,.F.);
#2220=ORIENTED_EDGE('',*,*,#1680,.F.);
#2221=ORIENTED_EDGE('',*,*,#1678,.F.);
#2222=ORIENTED_EDGE('',*,*,#1679,.T.);
#2223=ORIENTED_EDGE('',*,*,#1680,.T.);
#2224=ORIENTED_EDGE('',*,*,#1681,.T.);
#2225=ORIENTED_EDGE('',*,*,#1682,.T.);
#2226=ORIENTED_EDGE('',*,*,#1681,.F.);
#2227=ORIENTED_EDGE('',*,*,#1683,.T.);
#2228=ORIENTED_EDGE('',*,*,#1684,.T.);
#2229=ORIENTED_EDGE('',*,*,#1685,.F.);
#2230=ORIENTED_EDGE('',*,*,#1684,.F.);
#2231=ORIENTED_EDGE('',*,*,#1685,.T.);
#2232=ORIENTED_EDGE('',*,*,#1686,.T.);
#2233=ORIENTED_EDGE('',*,*,#1687,.F.);
#2234=ORIENTED_EDGE('',*,*,#1686,.F.);
#2235=ORIENTED_EDGE('',*,*,#1682,.F.);
#2236=ORIENTED_EDGE('',*,*,#1687,.T.);
#2237=ORIENTED_EDGE('',*,*,#1688,.F.);
#2238=ORIENTED_EDGE('',*,*,#1689,.T.);
#2239=ORIENTED_EDGE('',*,*,#1676,.T.);
#2240=ORIENTED_EDGE('',*,*,#1677,.T.);
#2241=ORIENTED_EDGE('',*,*,#1689,.F.);
#2242=ORIENTED_EDGE('',*,*,#1688,.T.);
#2243=ORIENTED_EDGE('',*,*,#1690,.F.);
#2244=ORIENTED_EDGE('',*,*,#1690,.T.);
#2245=ORIENTED_EDGE('',*,*,#1691,.T.);
#2246=ORIENTED_EDGE('',*,*,#1683,.F.);
#2247=ORIENTED_EDGE('',*,*,#1691,.F.);
#2248=ORIENTED_EDGE('',*,*,#1692,.F.);
#2249=ORIENTED_EDGE('',*,*,#1693,.F.);
#2250=ORIENTED_EDGE('',*,*,#1694,.T.);
#2251=ORIENTED_EDGE('',*,*,#1695,.F.);
#2252=ORIENTED_EDGE('',*,*,#1696,.F.);
#2253=ORIENTED_EDGE('',*,*,#1694,.F.);
#2254=ORIENTED_EDGE('',*,*,#1697,.T.);
#2255=ORIENTED_EDGE('',*,*,#1698,.T.);
#2256=ORIENTED_EDGE('',*,*,#1695,.T.);
#2257=ORIENTED_EDGE('',*,*,#1696,.T.);
#2258=ORIENTED_EDGE('',*,*,#1698,.F.);
#2259=ORIENTED_EDGE('',*,*,#1699,.F.);
#2260=ORIENTED_EDGE('',*,*,#1700,.T.);
#2261=ORIENTED_EDGE('',*,*,#1701,.F.);
#2262=ORIENTED_EDGE('',*,*,#1702,.T.);
#2263=ORIENTED_EDGE('',*,*,#1699,.T.);
#2264=ORIENTED_EDGE('',*,*,#1702,.F.);
#2265=ORIENTED_EDGE('',*,*,#1703,.F.);
#2266=ORIENTED_EDGE('',*,*,#1704,.T.);
#2267=ORIENTED_EDGE('',*,*,#1701,.T.);
#2268=ORIENTED_EDGE('',*,*,#1704,.F.);
#2269=ORIENTED_EDGE('',*,*,#1705,.F.);
#2270=ORIENTED_EDGE('',*,*,#1706,.T.);
#2271=ORIENTED_EDGE('',*,*,#1703,.T.);
#2272=ORIENTED_EDGE('',*,*,#1706,.F.);
#2273=ORIENTED_EDGE('',*,*,#1705,.T.);
#2274=ORIENTED_EDGE('',*,*,#1697,.F.);
#2275=ORIENTED_EDGE('',*,*,#1692,.T.);
#2276=ORIENTED_EDGE('',*,*,#1693,.T.);
#2277=ORIENTED_EDGE('',*,*,#1707,.T.);
#2278=ORIENTED_EDGE('',*,*,#1700,.F.);
#2279=ORIENTED_EDGE('',*,*,#1707,.F.);
#2280=ORIENTED_EDGE('',*,*,#1708,.T.);
#2281=ORIENTED_EDGE('',*,*,#1708,.F.);
#2282=ORIENTED_EDGE('',*,*,#1709,.T.);
#2283=ORIENTED_EDGE('',*,*,#1709,.F.);
#2284=ORIENTED_EDGE('',*,*,#1710,.T.);
#2285=ORIENTED_EDGE('',*,*,#1710,.F.);
#2286=ORIENTED_EDGE('',*,*,#1711,.T.);
#2287=ORIENTED_EDGE('',*,*,#1711,.F.);
#2288=ORIENTED_EDGE('',*,*,#1712,.T.);
#2289=ORIENTED_EDGE('',*,*,#1712,.F.);
#2290=ORIENTED_EDGE('',*,*,#1713,.T.);
#2291=ORIENTED_EDGE('',*,*,#1713,.F.);
#2292=ORIENTED_EDGE('',*,*,#1714,.T.);
#2293=ORIENTED_EDGE('',*,*,#1714,.F.);
#2294=ORIENTED_EDGE('',*,*,#1715,.T.);
#2295=ORIENTED_EDGE('',*,*,#1715,.F.);
#2296=ORIENTED_EDGE('',*,*,#1716,.F.);
#2297=ORIENTED_EDGE('',*,*,#1717,.F.);
#2298=ORIENTED_EDGE('',*,*,#1718,.F.);
#2299=ORIENTED_EDGE('',*,*,#1719,.F.);
#2300=ORIENTED_EDGE('',*,*,#1718,.T.);
#2301=ORIENTED_EDGE('',*,*,#1720,.F.);
#2302=ORIENTED_EDGE('',*,*,#1721,.T.);
#2303=ORIENTED_EDGE('',*,*,#1722,.F.);
#2304=ORIENTED_EDGE('',*,*,#1723,.T.);
#2305=ORIENTED_EDGE('',*,*,#1724,.F.);
#2306=ORIENTED_EDGE('',*,*,#1725,.T.);
#2307=ORIENTED_EDGE('',*,*,#1726,.T.);
#2308=ORIENTED_EDGE('',*,*,#1727,.F.);
#2309=ORIENTED_EDGE('',*,*,#1726,.F.);
#2310=ORIENTED_EDGE('',*,*,#1728,.T.);
#2311=ORIENTED_EDGE('',*,*,#1729,.F.);
#2312=ORIENTED_EDGE('',*,*,#1730,.T.);
#2313=ORIENTED_EDGE('',*,*,#1731,.F.);
#2314=ORIENTED_EDGE('',*,*,#1732,.T.);
#2315=ORIENTED_EDGE('',*,*,#1733,.F.);
#2316=ORIENTED_EDGE('',*,*,#1734,.T.);
#2317=ORIENTED_EDGE('',*,*,#1735,.F.);
#2318=ORIENTED_EDGE('',*,*,#1736,.T.);
#2319=ORIENTED_EDGE('',*,*,#1737,.F.);
#2320=ORIENTED_EDGE('',*,*,#1717,.T.);
#2321=ORIENTED_EDGE('',*,*,#1738,.T.);
#2322=ORIENTED_EDGE('',*,*,#1739,.T.);
#2323=ORIENTED_EDGE('',*,*,#1720,.T.);
#2324=ORIENTED_EDGE('',*,*,#1740,.F.);
#2325=ORIENTED_EDGE('',*,*,#1741,.F.);
#2326=ORIENTED_EDGE('',*,*,#1721,.F.);
#2327=ORIENTED_EDGE('',*,*,#1739,.F.);
#2328=ORIENTED_EDGE('',*,*,#1741,.T.);
#2329=ORIENTED_EDGE('',*,*,#1742,.T.);
#2330=ORIENTED_EDGE('',*,*,#1743,.T.);
#2331=ORIENTED_EDGE('',*,*,#1722,.T.);
#2332=ORIENTED_EDGE('',*,*,#1744,.F.);
#2333=ORIENTED_EDGE('',*,*,#1745,.F.);
#2334=ORIENTED_EDGE('',*,*,#1723,.F.);
#2335=ORIENTED_EDGE('',*,*,#1743,.F.);
#2336=ORIENTED_EDGE('',*,*,#1745,.T.);
#2337=ORIENTED_EDGE('',*,*,#1746,.T.);
#2338=ORIENTED_EDGE('',*,*,#1747,.T.);
#2339=ORIENTED_EDGE('',*,*,#1724,.T.);
#2340=ORIENTED_EDGE('',*,*,#1748,.F.);
#2341=ORIENTED_EDGE('',*,*,#1749,.F.);
#2342=ORIENTED_EDGE('',*,*,#1728,.F.);
#2343=ORIENTED_EDGE('',*,*,#1725,.F.);
#2344=ORIENTED_EDGE('',*,*,#1747,.F.);
#2345=ORIENTED_EDGE('',*,*,#1750,.F.);
#2346=ORIENTED_EDGE('',*,*,#1749,.T.);
#2347=ORIENTED_EDGE('',*,*,#1751,.T.);
#2348=ORIENTED_EDGE('',*,*,#1752,.T.);
#2349=ORIENTED_EDGE('',*,*,#1729,.T.);
#2350=ORIENTED_EDGE('',*,*,#1753,.F.);
#2351=ORIENTED_EDGE('',*,*,#1754,.F.);
#2352=ORIENTED_EDGE('',*,*,#1730,.F.);
#2353=ORIENTED_EDGE('',*,*,#1752,.F.);
#2354=ORIENTED_EDGE('',*,*,#1754,.T.);
#2355=ORIENTED_EDGE('',*,*,#1755,.T.);
#2356=ORIENTED_EDGE('',*,*,#1756,.T.);
#2357=ORIENTED_EDGE('',*,*,#1731,.T.);
#2358=ORIENTED_EDGE('',*,*,#1757,.F.);
#2359=ORIENTED_EDGE('',*,*,#1758,.F.);
#2360=ORIENTED_EDGE('',*,*,#1732,.F.);
#2361=ORIENTED_EDGE('',*,*,#1756,.F.);
#2362=ORIENTED_EDGE('',*,*,#1758,.T.);
#2363=ORIENTED_EDGE('',*,*,#1759,.T.);
#2364=ORIENTED_EDGE('',*,*,#1760,.T.);
#2365=ORIENTED_EDGE('',*,*,#1733,.T.);
#2366=ORIENTED_EDGE('',*,*,#1734,.F.);
#2367=ORIENTED_EDGE('',*,*,#1760,.F.);
#2368=ORIENTED_EDGE('',*,*,#1761,.F.);
#2369=ORIENTED_EDGE('',*,*,#1762,.F.);
#2370=ORIENTED_EDGE('',*,*,#1763,.F.);
#2371=ORIENTED_EDGE('',*,*,#1764,.T.);
#2372=ORIENTED_EDGE('',*,*,#1750,.T.);
#2373=ORIENTED_EDGE('',*,*,#1746,.F.);
#2374=ORIENTED_EDGE('',*,*,#1744,.T.);
#2375=ORIENTED_EDGE('',*,*,#1742,.F.);
#2376=ORIENTED_EDGE('',*,*,#1740,.T.);
#2377=ORIENTED_EDGE('',*,*,#1738,.F.);
#2378=ORIENTED_EDGE('',*,*,#1716,.T.);
#2379=ORIENTED_EDGE('',*,*,#1765,.F.);
#2380=ORIENTED_EDGE('',*,*,#1766,.T.);
#2381=ORIENTED_EDGE('',*,*,#1767,.F.);
#2382=ORIENTED_EDGE('',*,*,#1761,.T.);
#2383=ORIENTED_EDGE('',*,*,#1759,.F.);
#2384=ORIENTED_EDGE('',*,*,#1757,.T.);
#2385=ORIENTED_EDGE('',*,*,#1755,.F.);
#2386=ORIENTED_EDGE('',*,*,#1753,.T.);
#2387=ORIENTED_EDGE('',*,*,#1751,.F.);
#2388=ORIENTED_EDGE('',*,*,#1748,.T.);
#2389=ORIENTED_EDGE('',*,*,#1764,.F.);
#2390=ORIENTED_EDGE('',*,*,#1719,.T.);
#2391=ORIENTED_EDGE('',*,*,#1737,.T.);
#2392=ORIENTED_EDGE('',*,*,#1768,.T.);
#2393=ORIENTED_EDGE('',*,*,#1765,.T.);
#2394=ORIENTED_EDGE('',*,*,#1736,.F.);
#2395=ORIENTED_EDGE('',*,*,#1769,.F.);
#2396=ORIENTED_EDGE('',*,*,#1766,.F.);
#2397=ORIENTED_EDGE('',*,*,#1768,.F.);
#2398=ORIENTED_EDGE('',*,*,#1727,.T.);
#2399=ORIENTED_EDGE('',*,*,#1763,.T.);
#2400=ORIENTED_EDGE('',*,*,#1762,.T.);
#2401=ORIENTED_EDGE('',*,*,#1767,.T.);
#2402=ORIENTED_EDGE('',*,*,#1769,.T.);
#2403=ORIENTED_EDGE('',*,*,#1735,.T.);
#2404=ORIENTED_EDGE('',*,*,#1770,.F.);
#2405=ORIENTED_EDGE('',*,*,#1771,.T.);
#2406=ORIENTED_EDGE('',*,*,#1772,.F.);
#2407=ORIENTED_EDGE('',*,*,#1773,.T.);
#2408=ORIENTED_EDGE('',*,*,#1770,.T.);
#2409=ORIENTED_EDGE('',*,*,#1773,.F.);
#2410=ORIENTED_EDGE('',*,*,#1772,.T.);
#2411=ORIENTED_EDGE('',*,*,#1774,.F.);
#2412=ORIENTED_EDGE('',*,*,#1774,.T.);
#2413=ORIENTED_EDGE('',*,*,#1775,.T.);
#2414=ORIENTED_EDGE('',*,*,#1771,.F.);
#2415=ORIENTED_EDGE('',*,*,#1775,.F.);
#2416=ORIENTED_EDGE('',*,*,#1776,.F.);
#2417=ORIENTED_EDGE('',*,*,#1777,.T.);
#2418=ORIENTED_EDGE('',*,*,#1778,.F.);
#2419=ORIENTED_EDGE('',*,*,#1779,.T.);
#2420=ORIENTED_EDGE('',*,*,#1776,.T.);
#2421=ORIENTED_EDGE('',*,*,#1779,.F.);
#2422=ORIENTED_EDGE('',*,*,#1778,.T.);
#2423=ORIENTED_EDGE('',*,*,#1780,.F.);
#2424=ORIENTED_EDGE('',*,*,#1780,.T.);
#2425=ORIENTED_EDGE('',*,*,#1781,.T.);
#2426=ORIENTED_EDGE('',*,*,#1777,.F.);
#2427=ORIENTED_EDGE('',*,*,#1781,.F.);
#2428=CYLINDRICAL_SURFACE('',#2926,0.6);
#2429=CYLINDRICAL_SURFACE('',#2929,0.425);
#2430=CYLINDRICAL_SURFACE('',#2932,0.425);
#2431=CYLINDRICAL_SURFACE('',#2935,0.425);
#2432=CYLINDRICAL_SURFACE('',#2938,0.425);
#2433=CYLINDRICAL_SURFACE('',#2948,0.4);
#2434=CYLINDRICAL_SURFACE('',#2955,1.);
#2435=CYLINDRICAL_SURFACE('',#2958,0.6);
#2436=CYLINDRICAL_SURFACE('',#2962,0.605);
#2437=CYLINDRICAL_SURFACE('',#2965,2.);
#2438=CYLINDRICAL_SURFACE('',#2971,0.42);
#2439=CYLINDRICAL_SURFACE('',#2974,0.8);
#2440=CYLINDRICAL_SURFACE('',#2987,0.338975);
#2441=CYLINDRICAL_SURFACE('',#3002,0.8);
#2442=CYLINDRICAL_SURFACE('',#3005,0.5);
#2443=CYLINDRICAL_SURFACE('',#3008,0.5);
#2444=CYLINDRICAL_SURFACE('',#3026,0.605);
#2445=CYLINDRICAL_SURFACE('',#3029,0.8);
#2446=CYLINDRICAL_SURFACE('',#3035,0.8);
#2447=CYLINDRICAL_SURFACE('',#3038,2.);
#2448=CYLINDRICAL_SURFACE('',#3044,2.);
#2449=CYLINDRICAL_SURFACE('',#3047,2.2);
#2450=CYLINDRICAL_SURFACE('',#3053,0.165);
#2451=CYLINDRICAL_SURFACE('',#3060,0.8);
#2452=CYLINDRICAL_SURFACE('',#3063,0.5);
#2453=CYLINDRICAL_SURFACE('',#3067,0.505);
#2454=CYLINDRICAL_SURFACE('',#3070,0.7);
#2455=CYLINDRICAL_SURFACE('',#3076,0.505);
#2456=CYLINDRICAL_SURFACE('',#3079,0.7);
#2457=CYLINDRICAL_SURFACE('',#3085,0.225);
#2458=CYLINDRICAL_SURFACE('',#3088,0.8);
#2459=CYLINDRICAL_SURFACE('',#3108,0.35);
#2460=CYLINDRICAL_SURFACE('',#3116,0.1954);
#2461=CYLINDRICAL_SURFACE('',#3128,1.5);
#2462=CYLINDRICAL_SURFACE('',#3133,1.5);
#2463=CYLINDRICAL_SURFACE('',#3138,0.52);
#2464=CYLINDRICAL_SURFACE('',#3139,3.75);
#2465=CYLINDRICAL_SURFACE('',#3145,1.1);
#2466=CYLINDRICAL_SURFACE('',#3148,1.5);
#2467=CYLINDRICAL_SURFACE('',#3154,1.1);
#2468=CYLINDRICAL_SURFACE('',#3157,1.5);
#2469=CYLINDRICAL_SURFACE('',#3170,0.976185);
#2470=CYLINDRICAL_SURFACE('',#3172,0.5);
#2471=CYLINDRICAL_SURFACE('',#3178,0.976185);
#2472=CYLINDRICAL_SURFACE('',#3190,1.023815);
#2473=CYLINDRICAL_SURFACE('',#3197,1.5);
#2474=CYLINDRICAL_SURFACE('',#3202,1.023815);
#2475=CYLINDRICAL_SURFACE('',#3224,1.019052);
#2476=CYLINDRICAL_SURFACE('',#3264,0.980948);
#2477=CYLINDRICAL_SURFACE('',#3278,1.013815);
#2478=CYLINDRICAL_SURFACE('',#3282,0.991185);
#2479=CYLINDRICAL_SURFACE('',#3286,1.013815);
#2480=CYLINDRICAL_SURFACE('',#3290,0.991185);
#2481=ADVANCED_FACE('',(#421),#2428,.F.);
#2482=ADVANCED_FACE('',(#422),#2429,.F.);
#2483=ADVANCED_FACE('',(#423),#2430,.F.);
#2484=ADVANCED_FACE('',(#424),#2431,.F.);
#2485=ADVANCED_FACE('',(#425),#2432,.F.);
#2486=ADVANCED_FACE('',(#426),#333,.T.);
#2487=ADVANCED_FACE('',(#427),#334,.T.);
#2488=ADVANCED_FACE('',(#428),#335,.T.);
#2489=ADVANCED_FACE('',(#429),#336,.T.);
#2490=ADVANCED_FACE('',(#430,#281,#282,#283,#284,#285),#337,.T.);
#2491=ADVANCED_FACE('',(#431,#286,#287,#288,#289,#290),#338,.F.);
#2492=ADVANCED_FACE('',(#432),#2433,.T.);
#2493=ADVANCED_FACE('',(#433),#339,.F.);
#2494=ADVANCED_FACE('',(#434,#291),#340,.F.);
#2495=ADVANCED_FACE('',(#435),#2434,.T.);
#2496=ADVANCED_FACE('',(#436),#341,.T.);
#2497=ADVANCED_FACE('',(#437),#2435,.T.);
#2498=ADVANCED_FACE('',(#438,#292),#342,.F.);
#2499=ADVANCED_FACE('',(#439),#2436,.F.);
#2500=ADVANCED_FACE('',(#440),#2437,.T.);
#2501=ADVANCED_FACE('',(#441,#293),#343,.T.);
#2502=ADVANCED_FACE('',(#442,#294),#344,.F.);
#2503=ADVANCED_FACE('',(#443),#2438,.F.);
#2504=ADVANCED_FACE('',(#444),#2439,.T.);
#2505=ADVANCED_FACE('',(#445,#295),#345,.T.);
#2506=ADVANCED_FACE('',(#446,#296),#346,.F.);
#2507=ADVANCED_FACE('',(#447),#169,.T.);
#2508=ADVANCED_FACE('',(#448),#170,.T.);
#2509=ADVANCED_FACE('',(#449),#347,.T.);
#2510=ADVANCED_FACE('',(#450),#348,.T.);
#2511=ADVANCED_FACE('',(#451),#349,.T.);
#2512=ADVANCED_FACE('',(#452),#2440,.F.);
#2513=ADVANCED_FACE('',(#453),#350,.T.);
#2514=ADVANCED_FACE('',(#454),#351,.T.);
#2515=ADVANCED_FACE('',(#455),#352,.T.);
#2516=ADVANCED_FACE('',(#456,#297),#353,.T.);
#2517=ADVANCED_FACE('',(#457,#298),#354,.F.);
#2518=ADVANCED_FACE('',(#458),#2441,.F.);
#2519=ADVANCED_FACE('',(#459),#2442,.F.);
#2520=ADVANCED_FACE('',(#460),#2443,.F.);
#2521=ADVANCED_FACE('',(#461),#355,.T.);
#2522=ADVANCED_FACE('',(#462),#356,.T.);
#2523=ADVANCED_FACE('',(#463),#357,.T.);
#2524=ADVANCED_FACE('',(#464),#358,.T.);
#2525=ADVANCED_FACE('',(#465),#359,.T.);
#2526=ADVANCED_FACE('',(#466),#360,.T.);
#2527=ADVANCED_FACE('',(#467),#361,.F.);
#2528=ADVANCED_FACE('',(#468,#299),#362,.F.);
#2529=ADVANCED_FACE('',(#469),#363,.T.);
#2530=ADVANCED_FACE('',(#470),#364,.T.);
#2531=ADVANCED_FACE('',(#471),#365,.T.);
#2532=ADVANCED_FACE('',(#472),#366,.T.);
#2533=ADVANCED_FACE('',(#473),#367,.T.);
#2534=ADVANCED_FACE('',(#474,#300),#368,.T.);
#2535=ADVANCED_FACE('',(#475),#2444,.F.);
#2536=ADVANCED_FACE('',(#476),#2445,.T.);
#2537=ADVANCED_FACE('',(#477,#301),#369,.T.);
#2538=ADVANCED_FACE('',(#478,#302),#370,.F.);
#2539=ADVANCED_FACE('',(#479),#2446,.F.);
#2540=ADVANCED_FACE('',(#480),#2447,.T.);
#2541=ADVANCED_FACE('',(#481,#303),#371,.T.);
#2542=ADVANCED_FACE('',(#482,#304),#372,.F.);
#2543=ADVANCED_FACE('',(#483),#2448,.F.);
#2544=ADVANCED_FACE('',(#484),#2449,.T.);
#2545=ADVANCED_FACE('',(#485,#305),#373,.T.);
#2546=ADVANCED_FACE('',(#486,#306),#374,.F.);
#2547=ADVANCED_FACE('',(#487),#2450,.F.);
#2548=ADVANCED_FACE('',(#488),#375,.T.);
#2549=ADVANCED_FACE('',(#489,#307),#376,.T.);
#2550=ADVANCED_FACE('',(#490),#2451,.T.);
#2551=ADVANCED_FACE('',(#491),#377,.F.);
#2552=ADVANCED_FACE('',(#492),#2452,.T.);
#2553=ADVANCED_FACE('',(#493,#308),#378,.T.);
#2554=ADVANCED_FACE('',(#494),#2453,.F.);
#2555=ADVANCED_FACE('',(#495),#2454,.T.);
#2556=ADVANCED_FACE('',(#496,#309),#379,.T.);
#2557=ADVANCED_FACE('',(#497,#310),#380,.F.);
#2558=ADVANCED_FACE('',(#498),#2455,.F.);
#2559=ADVANCED_FACE('',(#499),#2456,.T.);
#2560=ADVANCED_FACE('',(#500,#311),#381,.T.);
#2561=ADVANCED_FACE('',(#501,#312),#382,.F.);
#2562=ADVANCED_FACE('',(#502),#2457,.F.);
#2563=ADVANCED_FACE('',(#503),#2458,.T.);
#2564=ADVANCED_FACE('',(#504,#313),#383,.T.);
#2565=ADVANCED_FACE('',(#505,#314),#384,.F.);
#2566=ADVANCED_FACE('',(#506),#385,.F.);
#2567=ADVANCED_FACE('',(#507),#386,.F.);
#2568=ADVANCED_FACE('',(#508),#387,.F.);
#2569=ADVANCED_FACE('',(#509),#388,.F.);
#2570=ADVANCED_FACE('',(#510),#389,.F.);
#2571=ADVANCED_FACE('',(#511),#390,.F.);
#2572=ADVANCED_FACE('',(#512),#391,.F.);
#2573=ADVANCED_FACE('',(#513),#392,.F.);
#2574=ADVANCED_FACE('',(#514),#393,.F.);
#2575=ADVANCED_FACE('',(#515),#394,.T.);
#2576=ADVANCED_FACE('',(#516),#171,.T.);
#2577=ADVANCED_FACE('',(#517),#2459,.T.);
#2578=ADVANCED_FACE('',(#518),#172,.T.);
#2579=ADVANCED_FACE('',(#519,#315),#395,.T.);
#2580=ADVANCED_FACE('',(#520),#173,.T.);
#2581=ADVANCED_FACE('',(#521),#2460,.T.);
#2582=ADVANCED_FACE('',(#522),#2461,.F.);
#2583=ADVANCED_FACE('',(#523,#316),#396,.T.);
#2584=ADVANCED_FACE('',(#524),#2462,.F.);
#2585=ADVANCED_FACE('',(#525,#317),#397,.F.);
#2586=ADVANCED_FACE('',(#526),#2463,.F.);
#2587=ADVANCED_FACE('',(#527),#2464,.T.);
#2588=ADVANCED_FACE('',(#528,#318),#398,.T.);
#2589=ADVANCED_FACE('',(#529,#319),#399,.F.);
#2590=ADVANCED_FACE('',(#530),#2465,.F.);
#2591=ADVANCED_FACE('',(#531),#2466,.T.);
#2592=ADVANCED_FACE('',(#532,#320),#400,.T.);
#2593=ADVANCED_FACE('',(#533,#321),#401,.F.);
#2594=ADVANCED_FACE('',(#534),#2467,.F.);
#2595=ADVANCED_FACE('',(#535),#2468,.T.);
#2596=ADVANCED_FACE('',(#536,#322),#402,.T.);
#2597=ADVANCED_FACE('',(#537,#323),#403,.F.);
#2598=ADVANCED_FACE('',(#538),#45,.F.);
#2599=ADVANCED_FACE('',(#539),#2469,.T.);
#2600=ADVANCED_FACE('',(#540),#2470,.F.);
#2601=ADVANCED_FACE('',(#541),#174,.F.);
#2602=ADVANCED_FACE('',(#542,#324),#404,.T.);
#2603=ADVANCED_FACE('',(#543),#2471,.T.);
#2604=ADVANCED_FACE('',(#544,#325),#405,.T.);
#2605=ADVANCED_FACE('',(#545),#175,.F.);
#2606=ADVANCED_FACE('',(#546),#46,.F.);
#2607=ADVANCED_FACE('',(#547),#2472,.F.);
#2608=ADVANCED_FACE('',(#548,#326),#406,.T.);
#2609=ADVANCED_FACE('',(#549),#176,.T.);
#2610=ADVANCED_FACE('',(#550),#2473,.T.);
#2611=ADVANCED_FACE('',(#551),#177,.T.);
#2612=ADVANCED_FACE('',(#552,#327),#407,.T.);
#2613=ADVANCED_FACE('',(#553),#2474,.F.);
#2614=ADVANCED_FACE('',(#554),#29,.T.);
#2615=ADVANCED_FACE('',(#555),#30,.T.);
#2616=ADVANCED_FACE('',(#556),#31,.T.);
#2617=ADVANCED_FACE('',(#557),#32,.T.);
#2618=ADVANCED_FACE('',(#558),#33,.T.);
#2619=ADVANCED_FACE('',(#559),#34,.T.);
#2620=ADVANCED_FACE('',(#560),#35,.T.);
#2621=ADVANCED_FACE('',(#561),#36,.T.);
#2622=ADVANCED_FACE('',(#562),#37,.F.);
#2623=ADVANCED_FACE('',(#563),#2475,.T.);
#2624=ADVANCED_FACE('',(#564),#408,.T.);
#2625=ADVANCED_FACE('',(#565),#38,.F.);
#2626=ADVANCED_FACE('',(#566),#409,.T.);
#2627=ADVANCED_FACE('',(#567),#39,.F.);
#2628=ADVANCED_FACE('',(#568),#410,.T.);
#2629=ADVANCED_FACE('',(#569),#40,.F.);
#2630=ADVANCED_FACE('',(#570),#411,.T.);
#2631=ADVANCED_FACE('',(#571),#41,.F.);
#2632=ADVANCED_FACE('',(#572),#412,.T.);
#2633=ADVANCED_FACE('',(#573),#42,.F.);
#2634=ADVANCED_FACE('',(#574),#413,.T.);
#2635=ADVANCED_FACE('',(#575),#43,.F.);
#2636=ADVANCED_FACE('',(#576),#2476,.F.);
#2637=ADVANCED_FACE('',(#577),#414,.T.);
#2638=ADVANCED_FACE('',(#578),#44,.F.);
#2639=ADVANCED_FACE('',(#579,#328),#415,.T.);
#2640=ADVANCED_FACE('',(#580),#416,.T.);
#2641=ADVANCED_FACE('',(#581,#329),#417,.T.);
#2642=ADVANCED_FACE('',(#582),#2477,.T.);
#2643=ADVANCED_FACE('',(#583,#330),#418,.T.);
#2644=ADVANCED_FACE('',(#584),#2478,.F.);
#2645=ADVANCED_FACE('',(#585,#331),#419,.T.);
#2646=ADVANCED_FACE('',(#586),#2479,.T.);
#2647=ADVANCED_FACE('',(#587,#332),#420,.T.);
#2648=ADVANCED_FACE('',(#588),#2480,.F.);
#2649=CLOSED_SHELL('',(#2481,#2482,#2483,#2484,#2485,#2486,#2487,#2488,
#2489,#2490,#2491));
#2650=CLOSED_SHELL('',(#2492,#2493,#2494,#2495,#2496,#2497,#2498));
#2651=CLOSED_SHELL('',(#2499,#2500,#2501,#2502));
#2652=CLOSED_SHELL('',(#2503,#2504,#2505,#2506));
#2653=CLOSED_SHELL('',(#2507,#2508,#2509,#2510,#2511,#2512,#2513,#2514,
#2515,#2516,#2517));
#2654=CLOSED_SHELL('',(#2518,#2519,#2520,#2521,#2522,#2523,#2524,#2525,
#2526,#2527,#2528,#2529,#2530,#2531,#2532,#2533,#2534));
#2655=CLOSED_SHELL('',(#2535,#2536,#2537,#2538));
#2656=CLOSED_SHELL('',(#2539,#2540,#2541,#2542));
#2657=CLOSED_SHELL('',(#2543,#2544,#2545,#2546));
#2658=CLOSED_SHELL('',(#2547,#2548,#2549,#2550,#2551,#2552,#2553));
#2659=CLOSED_SHELL('',(#2554,#2555,#2556,#2557));
#2660=CLOSED_SHELL('',(#2558,#2559,#2560,#2561));
#2661=CLOSED_SHELL('',(#2562,#2563,#2564,#2565));
#2662=CLOSED_SHELL('',(#2566,#2567,#2568,#2569,#2570,#2571,#2572,#2573));
#2663=CLOSED_SHELL('',(#2574,#2575,#2576,#2577,#2578,#2579,#2580,#2581));
#2664=CLOSED_SHELL('',(#2582,#2583,#2584,#2585,#2586,#2587,#2588,#2589));
#2665=CLOSED_SHELL('',(#2590,#2591,#2592,#2593));
#2666=CLOSED_SHELL('',(#2594,#2595,#2596,#2597));
#2667=CLOSED_SHELL('',(#2598,#2599,#2600,#2601,#2602,#2603,#2604,#2605));
#2668=CLOSED_SHELL('',(#2606,#2607,#2608,#2609,#2610,#2611,#2612,#2613));
#2669=CLOSED_SHELL('',(#2614));
#2670=CLOSED_SHELL('',(#2615));
#2671=CLOSED_SHELL('',(#2616));
#2672=CLOSED_SHELL('',(#2617));
#2673=CLOSED_SHELL('',(#2618));
#2674=CLOSED_SHELL('',(#2619));
#2675=CLOSED_SHELL('',(#2620));
#2676=CLOSED_SHELL('',(#2621));
#2677=CLOSED_SHELL('',(#2622,#2623,#2624,#2625,#2626,#2627,#2628,#2629,
#2630,#2631,#2632,#2633,#2634,#2635,#2636,#2637,#2638,#2639,#2640));
#2678=CLOSED_SHELL('',(#2641,#2642,#2643,#2644));
#2679=CLOSED_SHELL('',(#2645,#2646,#2647,#2648));
#2680=DERIVED_UNIT_ELEMENT(#2724,1.);
#2681=DERIVED_UNIT_ELEMENT(#5387,-3.);
#2682=DERIVED_UNIT_ELEMENT(#2724,1.);
#2683=DERIVED_UNIT_ELEMENT(#5387,-3.);
#2684=DERIVED_UNIT_ELEMENT(#2724,1.);
#2685=DERIVED_UNIT_ELEMENT(#5387,-3.);
#2686=DERIVED_UNIT_ELEMENT(#2724,1.);
#2687=DERIVED_UNIT_ELEMENT(#5387,-3.);
#2688=DERIVED_UNIT_ELEMENT(#2724,1.);
#2689=DERIVED_UNIT_ELEMENT(#5387,-3.);
#2690=DERIVED_UNIT_ELEMENT(#2724,1.);
#2691=DERIVED_UNIT_ELEMENT(#5387,-3.);
#2692=DERIVED_UNIT_ELEMENT(#2724,1.);
#2693=DERIVED_UNIT_ELEMENT(#5387,-3.);
#2694=DERIVED_UNIT_ELEMENT(#2724,1.);
#2695=DERIVED_UNIT_ELEMENT(#5387,-3.);
#2696=DERIVED_UNIT_ELEMENT(#2724,1.);
#2697=DERIVED_UNIT_ELEMENT(#5387,-3.);
#2698=DERIVED_UNIT_ELEMENT(#2724,1.);
#2699=DERIVED_UNIT_ELEMENT(#5387,-3.);
#2700=DERIVED_UNIT_ELEMENT(#2724,1.);
#2701=DERIVED_UNIT_ELEMENT(#5387,-3.);
#2702=DERIVED_UNIT_ELEMENT(#2724,1.);
#2703=DERIVED_UNIT_ELEMENT(#5387,-3.);
#2704=DERIVED_UNIT_ELEMENT(#2724,1.);
#2705=DERIVED_UNIT_ELEMENT(#5387,-3.);
#2706=DERIVED_UNIT_ELEMENT(#2724,1.);
#2707=DERIVED_UNIT_ELEMENT(#5387,-3.);
#2708=DERIVED_UNIT_ELEMENT(#2724,1.);
#2709=DERIVED_UNIT_ELEMENT(#5387,-3.);
#2710=DERIVED_UNIT_ELEMENT(#2724,1.);
#2711=DERIVED_UNIT_ELEMENT(#5387,-3.);
#2712=DERIVED_UNIT_ELEMENT(#2724,1.);
#2713=DERIVED_UNIT_ELEMENT(#5387,-3.);
#2714=DERIVED_UNIT_ELEMENT(#2724,1.);
#2715=DERIVED_UNIT_ELEMENT(#5387,-3.);
#2716=DERIVED_UNIT_ELEMENT(#2724,1.);
#2717=DERIVED_UNIT_ELEMENT(#5387,-3.);
#2718=DERIVED_UNIT_ELEMENT(#2724,1.);
#2719=DERIVED_UNIT_ELEMENT(#5387,-3.);
#2720=DERIVED_UNIT_ELEMENT(#2724,1.);
#2721=DERIVED_UNIT_ELEMENT(#5387,-3.);
#2722=DERIVED_UNIT_ELEMENT(#2724,1.);
#2723=DERIVED_UNIT_ELEMENT(#5387,-3.);
#2724=(
MASS_UNIT()
NAMED_UNIT(*)
SI_UNIT(.KILO.,.GRAM.)
);
#2725=DERIVED_UNIT((#2680,#2681));
#2726=DERIVED_UNIT((#2682,#2683));
#2727=DERIVED_UNIT((#2684,#2685));
#2728=DERIVED_UNIT((#2686,#2687));
#2729=DERIVED_UNIT((#2688,#2689));
#2730=DERIVED_UNIT((#2690,#2691));
#2731=DERIVED_UNIT((#2692,#2693));
#2732=DERIVED_UNIT((#2694,#2695));
#2733=DERIVED_UNIT((#2696,#2697));
#2734=DERIVED_UNIT((#2698,#2699));
#2735=DERIVED_UNIT((#2700,#2701));
#2736=DERIVED_UNIT((#2702,#2703));
#2737=DERIVED_UNIT((#2704,#2705));
#2738=DERIVED_UNIT((#2706,#2707));
#2739=DERIVED_UNIT((#2708,#2709));
#2740=DERIVED_UNIT((#2710,#2711));
#2741=DERIVED_UNIT((#2712,#2713));
#2742=DERIVED_UNIT((#2714,#2715));
#2743=DERIVED_UNIT((#2716,#2717));
#2744=DERIVED_UNIT((#2718,#2719));
#2745=DERIVED_UNIT((#2720,#2721));
#2746=DERIVED_UNIT((#2722,#2723));
#2747=MEASURE_REPRESENTATION_ITEM('density measure',
POSITIVE_RATIO_MEASURE(7850.),#2725);
#2748=MEASURE_REPRESENTATION_ITEM('density measure',
POSITIVE_RATIO_MEASURE(7850.),#2726);
#2749=MEASURE_REPRESENTATION_ITEM('density measure',
POSITIVE_RATIO_MEASURE(7850.),#2727);
#2750=MEASURE_REPRESENTATION_ITEM('density measure',
POSITIVE_RATIO_MEASURE(7850.),#2728);
#2751=MEASURE_REPRESENTATION_ITEM('density measure',
POSITIVE_RATIO_MEASURE(7850.),#2729);
#2752=MEASURE_REPRESENTATION_ITEM('density measure',
POSITIVE_RATIO_MEASURE(7850.),#2730);
#2753=MEASURE_REPRESENTATION_ITEM('density measure',
POSITIVE_RATIO_MEASURE(7850.),#2731);
#2754=MEASURE_REPRESENTATION_ITEM('density measure',
POSITIVE_RATIO_MEASURE(7850.),#2732);
#2755=MEASURE_REPRESENTATION_ITEM('density measure',
POSITIVE_RATIO_MEASURE(7850.),#2733);
#2756=MEASURE_REPRESENTATION_ITEM('density measure',
POSITIVE_RATIO_MEASURE(7850.),#2734);
#2757=MEASURE_REPRESENTATION_ITEM('density measure',
POSITIVE_RATIO_MEASURE(7850.),#2735);
#2758=MEASURE_REPRESENTATION_ITEM('density measure',
POSITIVE_RATIO_MEASURE(7850.),#2736);
#2759=MEASURE_REPRESENTATION_ITEM('density measure',
POSITIVE_RATIO_MEASURE(7850.),#2737);
#2760=MEASURE_REPRESENTATION_ITEM('density measure',
POSITIVE_RATIO_MEASURE(7850.),#2738);
#2761=MEASURE_REPRESENTATION_ITEM('density measure',
POSITIVE_RATIO_MEASURE(7850.),#2739);
#2762=MEASURE_REPRESENTATION_ITEM('density measure',
POSITIVE_RATIO_MEASURE(7850.),#2740);
#2763=MEASURE_REPRESENTATION_ITEM('density measure',
POSITIVE_RATIO_MEASURE(7850.),#2741);
#2764=MEASURE_REPRESENTATION_ITEM('density measure',
POSITIVE_RATIO_MEASURE(7850.),#2742);
#2765=MEASURE_REPRESENTATION_ITEM('density measure',
POSITIVE_RATIO_MEASURE(7850.),#2743);
#2766=MEASURE_REPRESENTATION_ITEM('density measure',
POSITIVE_RATIO_MEASURE(7850.),#2744);
#2767=MEASURE_REPRESENTATION_ITEM('density measure',
POSITIVE_RATIO_MEASURE(7850.),#2745);
#2768=MEASURE_REPRESENTATION_ITEM('density measure',
POSITIVE_RATIO_MEASURE(7850.),#2746);
#2769=PROPERTY_DEFINITION_REPRESENTATION(#2879,#2813);
#2770=PROPERTY_DEFINITION_REPRESENTATION(#2880,#2814);
#2771=PROPERTY_DEFINITION_REPRESENTATION(#2881,#2815);
#2772=PROPERTY_DEFINITION_REPRESENTATION(#2882,#2816);
#2773=PROPERTY_DEFINITION_REPRESENTATION(#2883,#2817);
#2774=PROPERTY_DEFINITION_REPRESENTATION(#2884,#2818);
#2775=PROPERTY_DEFINITION_REPRESENTATION(#2885,#2819);
#2776=PROPERTY_DEFINITION_REPRESENTATION(#2886,#2820);
#2777=PROPERTY_DEFINITION_REPRESENTATION(#2887,#2821);
#2778=PROPERTY_DEFINITION_REPRESENTATION(#2888,#2822);
#2779=PROPERTY_DEFINITION_REPRESENTATION(#2889,#2823);
#2780=PROPERTY_DEFINITION_REPRESENTATION(#2890,#2824);
#2781=PROPERTY_DEFINITION_REPRESENTATION(#2891,#2825);
#2782=PROPERTY_DEFINITION_REPRESENTATION(#2892,#2826);
#2783=PROPERTY_DEFINITION_REPRESENTATION(#2893,#2827);
#2784=PROPERTY_DEFINITION_REPRESENTATION(#2894,#2828);
#2785=PROPERTY_DEFINITION_REPRESENTATION(#2895,#2829);
#2786=PROPERTY_DEFINITION_REPRESENTATION(#2896,#2830);
#2787=PROPERTY_DEFINITION_REPRESENTATION(#2897,#2831);
#2788=PROPERTY_DEFINITION_REPRESENTATION(#2898,#2832);
#2789=PROPERTY_DEFINITION_REPRESENTATION(#2899,#2833);
#2790=PROPERTY_DEFINITION_REPRESENTATION(#2900,#2834);
#2791=PROPERTY_DEFINITION_REPRESENTATION(#2901,#2835);
#2792=PROPERTY_DEFINITION_REPRESENTATION(#2902,#2836);
#2793=PROPERTY_DEFINITION_REPRESENTATION(#2903,#2837);
#2794=PROPERTY_DEFINITION_REPRESENTATION(#2904,#2838);
#2795=PROPERTY_DEFINITION_REPRESENTATION(#2905,#2839);
#2796=PROPERTY_DEFINITION_REPRESENTATION(#2906,#2840);
#2797=PROPERTY_DEFINITION_REPRESENTATION(#2907,#2841);
#2798=PROPERTY_DEFINITION_REPRESENTATION(#2908,#2842);
#2799=PROPERTY_DEFINITION_REPRESENTATION(#2909,#2843);
#2800=PROPERTY_DEFINITION_REPRESENTATION(#2910,#2844);
#2801=PROPERTY_DEFINITION_REPRESENTATION(#2911,#2845);
#2802=PROPERTY_DEFINITION_REPRESENTATION(#2912,#2846);
#2803=PROPERTY_DEFINITION_REPRESENTATION(#2913,#2847);
#2804=PROPERTY_DEFINITION_REPRESENTATION(#2914,#2848);
#2805=PROPERTY_DEFINITION_REPRESENTATION(#2915,#2849);
#2806=PROPERTY_DEFINITION_REPRESENTATION(#2916,#2850);
#2807=PROPERTY_DEFINITION_REPRESENTATION(#2917,#2851);
#2808=PROPERTY_DEFINITION_REPRESENTATION(#2918,#2852);
#2809=PROPERTY_DEFINITION_REPRESENTATION(#2919,#2853);
#2810=PROPERTY_DEFINITION_REPRESENTATION(#2920,#2854);
#2811=PROPERTY_DEFINITION_REPRESENTATION(#2921,#2855);
#2812=PROPERTY_DEFINITION_REPRESENTATION(#2922,#2856);
#2813=REPRESENTATION('material name',(#2857),#5360);
#2814=REPRESENTATION('density',(#2747),#5360);
#2815=REPRESENTATION('material name',(#2858),#5361);
#2816=REPRESENTATION('density',(#2748),#5361);
#2817=REPRESENTATION('material name',(#2859),#5362);
#2818=REPRESENTATION('density',(#2749),#5362);
#2819=REPRESENTATION('material name',(#2860),#5363);
#2820=REPRESENTATION('density',(#2750),#5363);
#2821=REPRESENTATION('material name',(#2861),#5364);
#2822=REPRESENTATION('density',(#2751),#5364);
#2823=REPRESENTATION('material name',(#2862),#5366);
#2824=REPRESENTATION('density',(#2752),#5366);
#2825=REPRESENTATION('material name',(#2863),#5367);
#2826=REPRESENTATION('density',(#2753),#5367);
#2827=REPRESENTATION('material name',(#2864),#5368);
#2828=REPRESENTATION('density',(#2754),#5368);
#2829=REPRESENTATION('material name',(#2865),#5369);
#2830=REPRESENTATION('density',(#2755),#5369);
#2831=REPRESENTATION('material name',(#2866),#5370);
#2832=REPRESENTATION('density',(#2756),#5370);
#2833=REPRESENTATION('material name',(#2867),#5371);
#2834=REPRESENTATION('density',(#2757),#5371);
#2835=REPRESENTATION('material name',(#2868),#5372);
#2836=REPRESENTATION('density',(#2758),#5372);
#2837=REPRESENTATION('material name',(#2869),#5373);
#2838=REPRESENTATION('density',(#2759),#5373);
#2839=REPRESENTATION('material name',(#2870),#5374);
#2840=REPRESENTATION('density',(#2760),#5374);
#2841=REPRESENTATION('material name',(#2871),#5376);
#2842=REPRESENTATION('density',(#2761),#5376);
#2843=REPRESENTATION('material name',(#2872),#5377);
#2844=REPRESENTATION('density',(#2762),#5377);
#2845=REPRESENTATION('material name',(#2873),#5378);
#2846=REPRESENTATION('density',(#2763),#5378);
#2847=REPRESENTATION('material name',(#2874),#5380);
#2848=REPRESENTATION('density',(#2764),#5380);
#2849=REPRESENTATION('material name',(#2875),#5381);
#2850=REPRESENTATION('density',(#2765),#5381);
#2851=REPRESENTATION('material name',(#2876),#5382);
#2852=REPRESENTATION('density',(#2766),#5382);
#2853=REPRESENTATION('material name',(#2877),#5383);
#2854=REPRESENTATION('density',(#2767),#5383);
#2855=REPRESENTATION('material name',(#2878),#5384);
#2856=REPRESENTATION('density',(#2768),#5384);
#2857=DESCRIPTIVE_REPRESENTATION_ITEM('Steel','Steel');
#2858=DESCRIPTIVE_REPRESENTATION_ITEM('Steel','Steel');
#2859=DESCRIPTIVE_REPRESENTATION_ITEM('Steel','Steel');
#2860=DESCRIPTIVE_REPRESENTATION_ITEM('Steel','Steel');
#2861=DESCRIPTIVE_REPRESENTATION_ITEM('Steel','Steel');
#2862=DESCRIPTIVE_REPRESENTATION_ITEM('Steel','Steel');
#2863=DESCRIPTIVE_REPRESENTATION_ITEM('Steel','Steel');
#2864=DESCRIPTIVE_REPRESENTATION_ITEM('Steel','Steel');
#2865=DESCRIPTIVE_REPRESENTATION_ITEM('Steel','Steel');
#2866=DESCRIPTIVE_REPRESENTATION_ITEM('Steel','Steel');
#2867=DESCRIPTIVE_REPRESENTATION_ITEM('Steel','Steel');
#2868=DESCRIPTIVE_REPRESENTATION_ITEM('Steel','Steel');
#2869=DESCRIPTIVE_REPRESENTATION_ITEM('Steel','Steel');
#2870=DESCRIPTIVE_REPRESENTATION_ITEM('Steel','Steel');
#2871=DESCRIPTIVE_REPRESENTATION_ITEM('Steel','Steel');
#2872=DESCRIPTIVE_REPRESENTATION_ITEM('Steel','Steel');
#2873=DESCRIPTIVE_REPRESENTATION_ITEM('Steel','Steel');
#2874=DESCRIPTIVE_REPRESENTATION_ITEM('Steel','Steel');
#2875=DESCRIPTIVE_REPRESENTATION_ITEM('Steel','Steel');
#2876=DESCRIPTIVE_REPRESENTATION_ITEM('Steel','Steel');
#2877=DESCRIPTIVE_REPRESENTATION_ITEM('Steel','Steel');
#2878=DESCRIPTIVE_REPRESENTATION_ITEM('Steel','Steel');
#2879=PROPERTY_DEFINITION('material property','material name',#5501);
#2880=PROPERTY_DEFINITION('material property','density of part',#5501);
#2881=PROPERTY_DEFINITION('material property','material name',#5502);
#2882=PROPERTY_DEFINITION('material property','density of part',#5502);
#2883=PROPERTY_DEFINITION('material property','material name',#5503);
#2884=PROPERTY_DEFINITION('material property','density of part',#5503);
#2885=PROPERTY_DEFINITION('material property','material name',#5504);
#2886=PROPERTY_DEFINITION('material property','density of part',#5504);
#2887=PROPERTY_DEFINITION('material property','material name',#5505);
#2888=PROPERTY_DEFINITION('material property','density of part',#5505);
#2889=PROPERTY_DEFINITION('material property','material name',#5507);
#2890=PROPERTY_DEFINITION('material property','density of part',#5507);
#2891=PROPERTY_DEFINITION('material property','material name',#5508);
#2892=PROPERTY_DEFINITION('material property','density of part',#5508);
#2893=PROPERTY_DEFINITION('material property','material name',#5509);
#2894=PROPERTY_DEFINITION('material property','density of part',#5509);
#2895=PROPERTY_DEFINITION('material property','material name',#5510);
#2896=PROPERTY_DEFINITION('material property','density of part',#5510);
#2897=PROPERTY_DEFINITION('material property','material name',#5511);
#2898=PROPERTY_DEFINITION('material property','density of part',#5511);
#2899=PROPERTY_DEFINITION('material property','material name',#5512);
#2900=PROPERTY_DEFINITION('material property','density of part',#5512);
#2901=PROPERTY_DEFINITION('material property','material name',#5513);
#2902=PROPERTY_DEFINITION('material property','density of part',#5513);
#2903=PROPERTY_DEFINITION('material property','material name',#5514);
#2904=PROPERTY_DEFINITION('material property','density of part',#5514);
#2905=PROPERTY_DEFINITION('material property','material name',#5515);
#2906=PROPERTY_DEFINITION('material property','density of part',#5515);
#2907=PROPERTY_DEFINITION('material property','material name',#5517);
#2908=PROPERTY_DEFINITION('material property','density of part',#5517);
#2909=PROPERTY_DEFINITION('material property','material name',#5518);
#2910=PROPERTY_DEFINITION('material property','density of part',#5518);
#2911=PROPERTY_DEFINITION('material property','material name',#5519);
#2912=PROPERTY_DEFINITION('material property','density of part',#5519);
#2913=PROPERTY_DEFINITION('material property','material name',#5521);
#2914=PROPERTY_DEFINITION('material property','density of part',#5521);
#2915=PROPERTY_DEFINITION('material property','material name',#5522);
#2916=PROPERTY_DEFINITION('material property','density of part',#5522);
#2917=PROPERTY_DEFINITION('material property','material name',#5523);
#2918=PROPERTY_DEFINITION('material property','density of part',#5523);
#2919=PROPERTY_DEFINITION('material property','material name',#5524);
#2920=PROPERTY_DEFINITION('material property','density of part',#5524);
#2921=PROPERTY_DEFINITION('material property','material name',#5525);
#2922=PROPERTY_DEFINITION('material property','density of part',#5525);
#2923=AXIS2_PLACEMENT_3D('',#4200,#3304,#3305);
#2924=AXIS2_PLACEMENT_3D('',#4201,#3306,#3307);
#2925=AXIS2_PLACEMENT_3D('',#4202,#3308,#3309);
#2926=AXIS2_PLACEMENT_3D('',#4203,#3310,#3311);
#2927=AXIS2_PLACEMENT_3D('',#4205,#3312,#3313);
#2928=AXIS2_PLACEMENT_3D('',#4208,#3315,#3316);
#2929=AXIS2_PLACEMENT_3D('',#4209,#3317,#3318);
#2930=AXIS2_PLACEMENT_3D('',#4211,#3319,#3320);
#2931=AXIS2_PLACEMENT_3D('',#4214,#3322,#3323);
#2932=AXIS2_PLACEMENT_3D('',#4215,#3324,#3325);
#2933=AXIS2_PLACEMENT_3D('',#4217,#3326,#3327);
#2934=AXIS2_PLACEMENT_3D('',#4220,#3329,#3330);
#2935=AXIS2_PLACEMENT_3D('',#4221,#3331,#3332);
#2936=AXIS2_PLACEMENT_3D('',#4223,#3333,#3334);
#2937=AXIS2_PLACEMENT_3D('',#4226,#3336,#3337);
#2938=AXIS2_PLACEMENT_3D('',#4227,#3338,#3339);
#2939=AXIS2_PLACEMENT_3D('',#4229,#3340,#3341);
#2940=AXIS2_PLACEMENT_3D('',#4232,#3343,#3344);
#2941=AXIS2_PLACEMENT_3D('',#4233,#3345,#3346);
#2942=AXIS2_PLACEMENT_3D('',#4242,#3351,#3352);
#2943=AXIS2_PLACEMENT_3D('',#4248,#3356,#3357);
#2944=AXIS2_PLACEMENT_3D('',#4254,#3361,#3362);
#2945=AXIS2_PLACEMENT_3D('',#4257,#3365,#3366);
#2946=AXIS2_PLACEMENT_3D('',#4258,#3367,#3368);
#2947=AXIS2_PLACEMENT_3D('',#4259,#3369,#3370);
#2948=AXIS2_PLACEMENT_3D('',#4260,#3371,#3372);
#2949=AXIS2_PLACEMENT_3D('',#4262,#3373,#3374);
#2950=AXIS2_PLACEMENT_3D('',#4265,#3376,#3377);
#2951=AXIS2_PLACEMENT_3D('',#4266,#3378,#3379);
#2952=AXIS2_PLACEMENT_3D('',#4267,#3380,#3381);
#2953=AXIS2_PLACEMENT_3D('',#4269,#3382,#3383);
#2954=AXIS2_PLACEMENT_3D('',#4271,#3384,#3385);
#2955=AXIS2_PLACEMENT_3D('',#4272,#3386,#3387);
#2956=AXIS2_PLACEMENT_3D('',#4274,#3388,#3389);
#2957=AXIS2_PLACEMENT_3D('',#4276,#3391,#3392);
#2958=AXIS2_PLACEMENT_3D('',#4277,#3393,#3394);
#2959=AXIS2_PLACEMENT_3D('',#4280,#3396,#3397);
#2960=AXIS2_PLACEMENT_3D('',#4281,#3398,#3399);
#2961=AXIS2_PLACEMENT_3D('',#4282,#3400,#3401);
#2962=AXIS2_PLACEMENT_3D('',#4283,#3402,#3403);
#2963=AXIS2_PLACEMENT_3D('',#4285,#3404,#3405);
#2964=AXIS2_PLACEMENT_3D('',#4288,#3407,#3408);
#2965=AXIS2_PLACEMENT_3D('',#4289,#3409,#3410);
#2966=AXIS2_PLACEMENT_3D('',#4291,#3411,#3412);
#2967=AXIS2_PLACEMENT_3D('',#4294,#3414,#3415);
#2968=AXIS2_PLACEMENT_3D('',#4295,#3416,#3417);
#2969=AXIS2_PLACEMENT_3D('',#4296,#3418,#3419);
#2970=AXIS2_PLACEMENT_3D('',#4297,#3420,#3421);
#2971=AXIS2_PLACEMENT_3D('',#4298,#3422,#3423);
#2972=AXIS2_PLACEMENT_3D('',#4300,#3424,#3425);
#2973=AXIS2_PLACEMENT_3D('',#4303,#3427,#3428);
#2974=AXIS2_PLACEMENT_3D('',#4304,#3429,#3430);
#2975=AXIS2_PLACEMENT_3D('',#4306,#3431,#3432);
#2976=AXIS2_PLACEMENT_3D('',#4309,#3434,#3435);
#2977=AXIS2_PLACEMENT_3D('',#4310,#3436,#3437);
#2978=AXIS2_PLACEMENT_3D('',#4311,#3438,#3439);
#2979=AXIS2_PLACEMENT_3D('',#4312,#3440,#3441);
#2980=AXIS2_PLACEMENT_3D('',#4313,#3442,#3443);
#2981=AXIS2_PLACEMENT_3D('',#4325,#3445,#3446);
#2982=AXIS2_PLACEMENT_3D('',#4341,#3447,#3448);
#2983=AXIS2_PLACEMENT_3D('',#4343,#3449,#3450);
#2984=AXIS2_PLACEMENT_3D('',#4369,#3452,#3453);
#2985=AXIS2_PLACEMENT_3D('',#4372,#3456,#3457);
#2986=AXIS2_PLACEMENT_3D('',#4374,#3459,#3460);
#2987=AXIS2_PLACEMENT_3D('',#4376,#3462,#3463);
#2988=AXIS2_PLACEMENT_3D('',#4378,#3464,#3465);
#2989=AXIS2_PLACEMENT_3D('',#4381,#3467,#3468);
#2990=AXIS2_PLACEMENT_3D('',#4382,#3469,#3470);
#2991=AXIS2_PLACEMENT_3D('',#4384,#3472,#3473);
#2992=AXIS2_PLACEMENT_3D('',#4386,#3475,#3476);
#2993=AXIS2_PLACEMENT_3D('',#4387,#3477,#3478);
#2994=AXIS2_PLACEMENT_3D('',#4388,#3479,#3480);
#2995=AXIS2_PLACEMENT_3D('',#4389,#3481,#3482);
#2996=AXIS2_PLACEMENT_3D('',#4390,#3483,#3484);
#2997=AXIS2_PLACEMENT_3D('',#4391,#3485,#3486);
#2998=AXIS2_PLACEMENT_3D('',#4392,#3487,#3488);
#2999=AXIS2_PLACEMENT_3D('',#4393,#3489,#3490);
#3000=AXIS2_PLACEMENT_3D('',#4394,#3491,#3492);
#3001=AXIS2_PLACEMENT_3D('',#4395,#3493,#3494);
#3002=AXIS2_PLACEMENT_3D('',#4396,#3495,#3496);
#3003=AXIS2_PLACEMENT_3D('',#4398,#3497,#3498);
#3004=AXIS2_PLACEMENT_3D('',#4401,#3500,#3501);
#3005=AXIS2_PLACEMENT_3D('',#4402,#3502,#3503);
#3006=AXIS2_PLACEMENT_3D('',#4405,#3504,#3505);
#3007=AXIS2_PLACEMENT_3D('',#4409,#3507,#3508);
#3008=AXIS2_PLACEMENT_3D('',#4411,#3510,#3511);
#3009=AXIS2_PLACEMENT_3D('',#4416,#3513,#3514);
#3010=AXIS2_PLACEMENT_3D('',#4419,#3516,#3517);
#3011=AXIS2_PLACEMENT_3D('',#4420,#3518,#3519);
#3012=AXIS2_PLACEMENT_3D('',#4434,#3527,#3528);
#3013=AXIS2_PLACEMENT_3D('',#4438,#3531,#3532);
#3014=AXIS2_PLACEMENT_3D('',#4442,#3535,#3536);
#3015=AXIS2_PLACEMENT_3D('',#4456,#3544,#3545);
#3016=AXIS2_PLACEMENT_3D('',#4460,#3548,#3549);
#3017=AXIS2_PLACEMENT_3D('',#4464,#3552,#3553);
#3018=AXIS2_PLACEMENT_3D('',#4468,#3556,#3557);
#3019=AXIS2_PLACEMENT_3D('',#4475,#3562,#3563);
#3020=AXIS2_PLACEMENT_3D('',#4478,#3566,#3567);
#3021=AXIS2_PLACEMENT_3D('',#4482,#3570,#3571);
#3022=AXIS2_PLACEMENT_3D('',#4484,#3573,#3574);
#3023=AXIS2_PLACEMENT_3D('',#4485,#3575,#3576);
#3024=AXIS2_PLACEMENT_3D('',#4487,#3578,#3579);
#3025=AXIS2_PLACEMENT_3D('',#4488,#3580,#3581);
#3026=AXIS2_PLACEMENT_3D('',#4489,#3582,#3583);
#3027=AXIS2_PLACEMENT_3D('',#4491,#3584,#3585);
#3028=AXIS2_PLACEMENT_3D('',#4494,#3587,#3588);
#3029=AXIS2_PLACEMENT_3D('',#4495,#3589,#3590);
#3030=AXIS2_PLACEMENT_3D('',#4497,#3591,#3592);
#3031=AXIS2_PLACEMENT_3D('',#4500,#3594,#3595);
#3032=AXIS2_PLACEMENT_3D('',#4501,#3596,#3597);
#3033=AXIS2_PLACEMENT_3D('',#4502,#3598,#3599);
#3034=AXIS2_PLACEMENT_3D('',#4503,#3600,#3601);
#3035=AXIS2_PLACEMENT_3D('',#4504,#3602,#3603);
#3036=AXIS2_PLACEMENT_3D('',#4506,#3604,#3605);
#3037=AXIS2_PLACEMENT_3D('',#4509,#3607,#3608);
#3038=AXIS2_PLACEMENT_3D('',#4510,#3609,#3610);
#3039=AXIS2_PLACEMENT_3D('',#4512,#3611,#3612);
#3040=AXIS2_PLACEMENT_3D('',#4515,#3614,#3615);
#3041=AXIS2_PLACEMENT_3D('',#4516,#3616,#3617);
#3042=AXIS2_PLACEMENT_3D('',#4517,#3618,#3619);
#3043=AXIS2_PLACEMENT_3D('',#4518,#3620,#3621);
#3044=AXIS2_PLACEMENT_3D('',#4519,#3622,#3623);
#3045=AXIS2_PLACEMENT_3D('',#4521,#3624,#3625);
#3046=AXIS2_PLACEMENT_3D('',#4524,#3627,#3628);
#3047=AXIS2_PLACEMENT_3D('',#4525,#3629,#3630);
#3048=AXIS2_PLACEMENT_3D('',#4527,#3631,#3632);
#3049=AXIS2_PLACEMENT_3D('',#4530,#3634,#3635);
#3050=AXIS2_PLACEMENT_3D('',#4531,#3636,#3637);
#3051=AXIS2_PLACEMENT_3D('',#4532,#3638,#3639);
#3052=AXIS2_PLACEMENT_3D('',#4533,#3640,#3641);
#3053=AXIS2_PLACEMENT_3D('',#4534,#3642,#3643);
#3054=AXIS2_PLACEMENT_3D('',#4536,#3644,#3645);
#3055=AXIS2_PLACEMENT_3D('',#4539,#3647,#3648);
#3056=AXIS2_PLACEMENT_3D('',#4540,#3649,#3650);
#3057=AXIS2_PLACEMENT_3D('',#4541,#3651,#3652);
#3058=AXIS2_PLACEMENT_3D('',#4543,#3653,#3654);
#3059=AXIS2_PLACEMENT_3D('',#4545,#3655,#3656);
#3060=AXIS2_PLACEMENT_3D('',#4546,#3657,#3658);
#3061=AXIS2_PLACEMENT_3D('',#4549,#3660,#3661);
#3062=AXIS2_PLACEMENT_3D('',#4550,#3662,#3663);
#3063=AXIS2_PLACEMENT_3D('',#4551,#3664,#3665);
#3064=AXIS2_PLACEMENT_3D('',#4553,#3666,#3667);
#3065=AXIS2_PLACEMENT_3D('',#4555,#3669,#3670);
#3066=AXIS2_PLACEMENT_3D('',#4556,#3671,#3672);
#3067=AXIS2_PLACEMENT_3D('',#4557,#3673,#3674);
#3068=AXIS2_PLACEMENT_3D('',#4559,#3675,#3676);
#3069=AXIS2_PLACEMENT_3D('',#4562,#3678,#3679);
#3070=AXIS2_PLACEMENT_3D('',#4563,#3680,#3681);
#3071=AXIS2_PLACEMENT_3D('',#4565,#3682,#3683);
#3072=AXIS2_PLACEMENT_3D('',#4568,#3685,#3686);
#3073=AXIS2_PLACEMENT_3D('',#4569,#3687,#3688);
#3074=AXIS2_PLACEMENT_3D('',#4570,#3689,#3690);
#3075=AXIS2_PLACEMENT_3D('',#4571,#3691,#3692);
#3076=AXIS2_PLACEMENT_3D('',#4572,#3693,#3694);
#3077=AXIS2_PLACEMENT_3D('',#4574,#3695,#3696);
#3078=AXIS2_PLACEMENT_3D('',#4577,#3698,#3699);
#3079=AXIS2_PLACEMENT_3D('',#4578,#3700,#3701);
#3080=AXIS2_PLACEMENT_3D('',#4580,#3702,#3703);
#3081=AXIS2_PLACEMENT_3D('',#4583,#3705,#3706);
#3082=AXIS2_PLACEMENT_3D('',#4584,#3707,#3708);
#3083=AXIS2_PLACEMENT_3D('',#4585,#3709,#3710);
#3084=AXIS2_PLACEMENT_3D('',#4586,#3711,#3712);
#3085=AXIS2_PLACEMENT_3D('',#4587,#3713,#3714);
#3086=AXIS2_PLACEMENT_3D('',#4589,#3715,#3716);
#3087=AXIS2_PLACEMENT_3D('',#4592,#3718,#3719);
#3088=AXIS2_PLACEMENT_3D('',#4593,#3720,#3721);
#3089=AXIS2_PLACEMENT_3D('',#4595,#3722,#3723);
#3090=AXIS2_PLACEMENT_3D('',#4598,#3725,#3726);
#3091=AXIS2_PLACEMENT_3D('',#4599,#3727,#3728);
#3092=AXIS2_PLACEMENT_3D('',#4600,#3729,#3730);
#3093=AXIS2_PLACEMENT_3D('',#4601,#3731,#3732);
#3094=AXIS2_PLACEMENT_3D('',#4602,#3733,#3734);
#3095=AXIS2_PLACEMENT_3D('',#4611,#3739,#3740);
#3096=AXIS2_PLACEMENT_3D('',#4617,#3744,#3745);
#3097=AXIS2_PLACEMENT_3D('',#4623,#3749,#3750);
#3098=AXIS2_PLACEMENT_3D('',#4629,#3754,#3755);
#3099=AXIS2_PLACEMENT_3D('',#4635,#3759,#3760);
#3100=AXIS2_PLACEMENT_3D('',#4638,#3763,#3764);
#3101=AXIS2_PLACEMENT_3D('',#4639,#3765,#3766);
#3102=AXIS2_PLACEMENT_3D('',#4640,#3767,#3768);
#3103=AXIS2_PLACEMENT_3D('',#4642,#3769,#3770);
#3104=AXIS2_PLACEMENT_3D('',#4643,#3771,#3772);
#3105=AXIS2_PLACEMENT_3D('',#4645,#3773,#3774);
#3106=AXIS2_PLACEMENT_3D('',#4646,#3775,#3776);
#3107=AXIS2_PLACEMENT_3D('',#4648,#3777,#3778);
#3108=AXIS2_PLACEMENT_3D('',#4650,#3780,#3781);
#3109=AXIS2_PLACEMENT_3D('',#4652,#3782,#3783);
#3110=AXIS2_PLACEMENT_3D('',#4654,#3785,#3786);
#3111=AXIS2_PLACEMENT_3D('',#4656,#3787,#3788);
#3112=AXIS2_PLACEMENT_3D('',#4658,#3790,#3791);
#3113=AXIS2_PLACEMENT_3D('',#4660,#3792,#3793);
#3114=AXIS2_PLACEMENT_3D('',#4661,#3794,#3795);
#3115=AXIS2_PLACEMENT_3D('',#4663,#3796,#3797);
#3116=AXIS2_PLACEMENT_3D('',#4665,#3799,#3800);
#3117=AXIS2_PLACEMENT_3D('',#4667,#3802,#3803);
#3118=AXIS2_PLACEMENT_3D('',#4668,#3804,#3805);
#3119=AXIS2_PLACEMENT_3D('',#4669,#3806,#3807);
#3120=AXIS2_PLACEMENT_3D('',#4670,#3808,#3809);
#3121=AXIS2_PLACEMENT_3D('',#4671,#3810,#3811);
#3122=AXIS2_PLACEMENT_3D('',#4672,#3812,#3813);
#3123=AXIS2_PLACEMENT_3D('',#4673,#3814,#3815);
#3124=AXIS2_PLACEMENT_3D('',#4674,#3816,#3817);
#3125=AXIS2_PLACEMENT_3D('',#4675,#3818,#3819);
#3126=AXIS2_PLACEMENT_3D('',#4676,#3820,#3821);
#3127=AXIS2_PLACEMENT_3D('',#4677,#3822,#3823);
#3128=AXIS2_PLACEMENT_3D('',#4678,#3824,#3825);
#3129=AXIS2_PLACEMENT_3D('',#4680,#3826,#3827);
#3130=AXIS2_PLACEMENT_3D('',#4683,#3829,#3830);
#3131=AXIS2_PLACEMENT_3D('',#4684,#3831,#3832);
#3132=AXIS2_PLACEMENT_3D('',#4686,#3833,#3834);
#3133=AXIS2_PLACEMENT_3D('',#4687,#3835,#3836);
#3134=AXIS2_PLACEMENT_3D('',#4689,#3837,#3838);
#3135=AXIS2_PLACEMENT_3D('',#4692,#3840,#3841);
#3136=AXIS2_PLACEMENT_3D('',#4693,#3842,#3843);
#3137=AXIS2_PLACEMENT_3D('',#4695,#3844,#3845);
#3138=AXIS2_PLACEMENT_3D('',#4696,#3846,#3847);
#3139=AXIS2_PLACEMENT_3D('',#4698,#3849,#3850);
#3140=AXIS2_PLACEMENT_3D('',#4700,#3851,#3852);
#3141=AXIS2_PLACEMENT_3D('',#4703,#3854,#3855);
#3142=AXIS2_PLACEMENT_3D('',#4704,#3856,#3857);
#3143=AXIS2_PLACEMENT_3D('',#4705,#3858,#3859);
#3144=AXIS2_PLACEMENT_3D('',#4706,#3860,#3861);
#3145=AXIS2_PLACEMENT_3D('',#4707,#3862,#3863);
#3146=AXIS2_PLACEMENT_3D('',#4709,#3864,#3865);
#3147=AXIS2_PLACEMENT_3D('',#4712,#3867,#3868);
#3148=AXIS2_PLACEMENT_3D('',#4713,#3869,#3870);
#3149=AXIS2_PLACEMENT_3D('',#4715,#3871,#3872);
#3150=AXIS2_PLACEMENT_3D('',#4718,#3874,#3875);
#3151=AXIS2_PLACEMENT_3D('',#4719,#3876,#3877);
#3152=AXIS2_PLACEMENT_3D('',#4720,#3878,#3879);
#3153=AXIS2_PLACEMENT_3D('',#4721,#3880,#3881);
#3154=AXIS2_PLACEMENT_3D('',#4722,#3882,#3883);
#3155=AXIS2_PLACEMENT_3D('',#4724,#3884,#3885);
#3156=AXIS2_PLACEMENT_3D('',#4727,#3887,#3888);
#3157=AXIS2_PLACEMENT_3D('',#4728,#3889,#3890);
#3158=AXIS2_PLACEMENT_3D('',#4730,#3891,#3892);
#3159=AXIS2_PLACEMENT_3D('',#4733,#3894,#3895);
#3160=AXIS2_PLACEMENT_3D('',#4734,#3896,#3897);
#3161=AXIS2_PLACEMENT_3D('',#4735,#3898,#3899);
#3162=AXIS2_PLACEMENT_3D('',#4736,#3900,#3901);
#3163=AXIS2_PLACEMENT_3D('',#4737,#3902,#3903);
#3164=AXIS2_PLACEMENT_3D('',#4738,#3904,#3905);
#3165=AXIS2_PLACEMENT_3D('',#4741,#3906,#3907);
#3166=AXIS2_PLACEMENT_3D('',#4742,#3908,#3909);
#3167=AXIS2_PLACEMENT_3D('',#4744,#3910,#3911);
#3168=AXIS2_PLACEMENT_3D('',#4746,#3912,#3913);
#3169=AXIS2_PLACEMENT_3D('',#4747,#3914,#3915);
#3170=AXIS2_PLACEMENT_3D('',#4748,#3916,#3917);
#3171=AXIS2_PLACEMENT_3D('',#4751,#3919,#3920);
#3172=AXIS2_PLACEMENT_3D('',#4752,#3921,#3922);
#3173=AXIS2_PLACEMENT_3D('',#4754,#3923,#3924);
#3174=AXIS2_PLACEMENT_3D('',#4757,#3926,#3927);
#3175=AXIS2_PLACEMENT_3D('',#4758,#3928,#3929);
#3176=AXIS2_PLACEMENT_3D('',#4761,#3931,#3932);
#3177=AXIS2_PLACEMENT_3D('',#4762,#3933,#3934);
#3178=AXIS2_PLACEMENT_3D('',#4763,#3935,#3936);
#3179=AXIS2_PLACEMENT_3D('',#4765,#3937,#3938);
#3180=AXIS2_PLACEMENT_3D('',#4767,#3940,#3941);
#3181=AXIS2_PLACEMENT_3D('',#4769,#3942,#3943);
#3182=AXIS2_PLACEMENT_3D('',#4770,#3944,#3945);
#3183=AXIS2_PLACEMENT_3D('',#4772,#3947,#3948);
#3184=AXIS2_PLACEMENT_3D('',#4773,#3949,#3950);
#3185=AXIS2_PLACEMENT_3D('',#4776,#3951,#3952);
#3186=AXIS2_PLACEMENT_3D('',#4777,#3953,#3954);
#3187=AXIS2_PLACEMENT_3D('',#4779,#3955,#3956);
#3188=AXIS2_PLACEMENT_3D('',#4781,#3957,#3958);
#3189=AXIS2_PLACEMENT_3D('',#4782,#3959,#3960);
#3190=AXIS2_PLACEMENT_3D('',#4783,#3961,#3962);
#3191=AXIS2_PLACEMENT_3D('',#4785,#3963,#3964);
#3192=AXIS2_PLACEMENT_3D('',#4787,#3966,#3967);
#3193=AXIS2_PLACEMENT_3D('',#4789,#3968,#3969);
#3194=AXIS2_PLACEMENT_3D('',#4791,#3970,#3971);
#3195=AXIS2_PLACEMENT_3D('',#4792,#3972,#3973);
#3196=AXIS2_PLACEMENT_3D('',#4794,#3974,#3975);
#3197=AXIS2_PLACEMENT_3D('',#4796,#3977,#3978);
#3198=AXIS2_PLACEMENT_3D('',#4798,#3979,#3980);
#3199=AXIS2_PLACEMENT_3D('',#4800,#3982,#3983);
#3200=AXIS2_PLACEMENT_3D('',#4802,#3984,#3985);
#3201=AXIS2_PLACEMENT_3D('',#4804,#3987,#3988);
#3202=AXIS2_PLACEMENT_3D('',#4805,#3989,#3990);
#3203=AXIS2_PLACEMENT_3D('',#4807,#3992,#3993);
#3204=AXIS2_PLACEMENT_3D('',#4808,#3994,#3995);
#3205=AXIS2_PLACEMENT_3D('',#4811,#3996,#3997);
#3206=AXIS2_PLACEMENT_3D('',#4812,#3998,#3999);
#3207=AXIS2_PLACEMENT_3D('',#4815,#4000,#4001);
#3208=AXIS2_PLACEMENT_3D('',#4816,#4002,#4003);
#3209=AXIS2_PLACEMENT_3D('',#4819,#4004,#4005);
#3210=AXIS2_PLACEMENT_3D('',#4820,#4006,#4007);
#3211=AXIS2_PLACEMENT_3D('',#4823,#4008,#4009);
#3212=AXIS2_PLACEMENT_3D('',#4824,#4010,#4011);
#3213=AXIS2_PLACEMENT_3D('',#4827,#4012,#4013);
#3214=AXIS2_PLACEMENT_3D('',#4828,#4014,#4015);
#3215=AXIS2_PLACEMENT_3D('',#4831,#4016,#4017);
#3216=AXIS2_PLACEMENT_3D('',#4832,#4018,#4019);
#3217=AXIS2_PLACEMENT_3D('',#4835,#4020,#4021);
#3218=AXIS2_PLACEMENT_3D('',#4836,#4022,#4023);
#3219=AXIS2_PLACEMENT_3D('',#4839,#4024,#4025);
#3220=AXIS2_PLACEMENT_3D('',#4840,#4026,#4027);
#3221=AXIS2_PLACEMENT_3D('',#4841,#4028,#4029);
#3222=AXIS2_PLACEMENT_3D('',#4867,#4030,#4031);
#3223=AXIS2_PLACEMENT_3D('',#4891,#4032,#4033);
#3224=AXIS2_PLACEMENT_3D('',#4892,#4034,#4035);
#3225=AXIS2_PLACEMENT_3D('',#4894,#4036,#4037);
#3226=AXIS2_PLACEMENT_3D('',#4919,#4038,#4039);
#3227=AXIS2_PLACEMENT_3D('',#4944,#4040,#4041);
#3228=AXIS2_PLACEMENT_3D('',#4960,#4043,#4044);
#3229=AXIS2_PLACEMENT_3D('',#4975,#4045,#4046);
#3230=AXIS2_PLACEMENT_3D('',#5000,#4047,#4048);
#3231=AXIS2_PLACEMENT_3D('',#5025,#4049,#4050);
#3232=AXIS2_PLACEMENT_3D('',#5050,#4051,#4052);
#3233=AXIS2_PLACEMENT_3D('',#5074,#4053,#4054);
#3234=AXIS2_PLACEMENT_3D('',#5075,#4055,#4056);
#3235=AXIS2_PLACEMENT_3D('',#5077,#4057,#4058);
#3236=AXIS2_PLACEMENT_3D('',#5078,#4059,#4060);
#3237=AXIS2_PLACEMENT_3D('',#5079,#4061,#4062);
#3238=AXIS2_PLACEMENT_3D('',#5103,#4063,#4064);
#3239=AXIS2_PLACEMENT_3D('',#5104,#4065,#4066);
#3240=AXIS2_PLACEMENT_3D('',#5106,#4067,#4068);
#3241=AXIS2_PLACEMENT_3D('',#5107,#4069,#4070);
#3242=AXIS2_PLACEMENT_3D('',#5108,#4071,#4072);
#3243=AXIS2_PLACEMENT_3D('',#5132,#4073,#4074);
#3244=AXIS2_PLACEMENT_3D('',#5133,#4075,#4076);
#3245=AXIS2_PLACEMENT_3D('',#5135,#4077,#4078);
#3246=AXIS2_PLACEMENT_3D('',#5136,#4079,#4080);
#3247=AXIS2_PLACEMENT_3D('',#5137,#4081,#4082);
#3248=AXIS2_PLACEMENT_3D('',#5152,#4083,#4084);
#3249=AXIS2_PLACEMENT_3D('',#5165,#4085,#4086);
#3250=AXIS2_PLACEMENT_3D('',#5167,#4087,#4088);
#3251=AXIS2_PLACEMENT_3D('',#5168,#4089,#4090);
#3252=AXIS2_PLACEMENT_3D('',#5169,#4091,#4092);
#3253=AXIS2_PLACEMENT_3D('',#5193,#4093,#4094);
#3254=AXIS2_PLACEMENT_3D('',#5194,#4095,#4096);
#3255=AXIS2_PLACEMENT_3D('',#5196,#4097,#4098);
#3256=AXIS2_PLACEMENT_3D('',#5197,#4099,#4100);
#3257=AXIS2_PLACEMENT_3D('',#5198,#4101,#4102);
#3258=AXIS2_PLACEMENT_3D('',#5222,#4103,#4104);
#3259=AXIS2_PLACEMENT_3D('',#5223,#4105,#4106);
#3260=AXIS2_PLACEMENT_3D('',#5225,#4107,#4108);
#3261=AXIS2_PLACEMENT_3D('',#5226,#4109,#4110);
#3262=AXIS2_PLACEMENT_3D('',#5227,#4111,#4112);
#3263=AXIS2_PLACEMENT_3D('',#5251,#4113,#4114);
#3264=AXIS2_PLACEMENT_3D('',#5252,#4115,#4116);
#3265=AXIS2_PLACEMENT_3D('',#5254,#4117,#4118);
#3266=AXIS2_PLACEMENT_3D('',#5257,#4120,#4121);
#3267=AXIS2_PLACEMENT_3D('',#5281,#4122,#4123);
#3268=AXIS2_PLACEMENT_3D('',#5282,#4124,#4125);
#3269=AXIS2_PLACEMENT_3D('',#5283,#4126,#4127);
#3270=AXIS2_PLACEMENT_3D('',#5284,#4128,#4129);
#3271=AXIS2_PLACEMENT_3D('',#5285,#4130,#4131);
#3272=AXIS2_PLACEMENT_3D('',#5286,#4132,#4133);
#3273=AXIS2_PLACEMENT_3D('',#5287,#4134,#4135);
#3274=AXIS2_PLACEMENT_3D('',#5288,#4136,#4137);
#3275=AXIS2_PLACEMENT_3D('',#5289,#4138,#4139);
#3276=AXIS2_PLACEMENT_3D('',#5291,#4140,#4141);
#3277=AXIS2_PLACEMENT_3D('',#5293,#4142,#4143);
#3278=AXIS2_PLACEMENT_3D('',#5294,#4144,#4145);
#3279=AXIS2_PLACEMENT_3D('',#5296,#4146,#4147);
#3280=AXIS2_PLACEMENT_3D('',#5298,#4149,#4150);
#3281=AXIS2_PLACEMENT_3D('',#5300,#4151,#4152);
#3282=AXIS2_PLACEMENT_3D('',#5301,#4153,#4154);
#3283=AXIS2_PLACEMENT_3D('',#5303,#4156,#4157);
#3284=AXIS2_PLACEMENT_3D('',#5305,#4158,#4159);
#3285=AXIS2_PLACEMENT_3D('',#5307,#4160,#4161);
#3286=AXIS2_PLACEMENT_3D('',#5308,#4162,#4163);
#3287=AXIS2_PLACEMENT_3D('',#5310,#4164,#4165);
#3288=AXIS2_PLACEMENT_3D('',#5312,#4167,#4168);
#3289=AXIS2_PLACEMENT_3D('',#5314,#4169,#4170);
#3290=AXIS2_PLACEMENT_3D('',#5315,#4171,#4172);
#3291=AXIS2_PLACEMENT_3D('',#5317,#4174,#4175);
#3292=AXIS2_PLACEMENT_3D('',#5318,#4176,#4177);
#3293=AXIS2_PLACEMENT_3D('',#5319,#4178,#4179);
#3294=AXIS2_PLACEMENT_3D('',#5320,#4180,#4181);
#3295=AXIS2_PLACEMENT_3D('',#5321,#4182,#4183);
#3296=AXIS2_PLACEMENT_3D('',#5322,#4184,#4185);
#3297=AXIS2_PLACEMENT_3D('',#5323,#4186,#4187);
#3298=AXIS2_PLACEMENT_3D('',#5324,#4188,#4189);
#3299=AXIS2_PLACEMENT_3D('',#5325,#4190,#4191);
#3300=AXIS2_PLACEMENT_3D('',#5326,#4192,#4193);
#3301=AXIS2_PLACEMENT_3D('',#5327,#4194,#4195);
#3302=AXIS2_PLACEMENT_3D('',#5328,#4196,#4197);
#3303=AXIS2_PLACEMENT_3D('',#5329,#4198,#4199);
#3304=DIRECTION('axis',(0.,0.,1.));
#3305=DIRECTION('refdir',(1.,0.,0.));
#3306=DIRECTION('axis',(0.,0.,1.));
#3307=DIRECTION('refdir',(1.,0.,0.));
#3308=DIRECTION('axis',(0.,0.,1.));
#3309=DIRECTION('refdir',(1.,0.,0.));
#3310=DIRECTION('center_axis',(0.,0.,1.));
#3311=DIRECTION('ref_axis',(1.,0.,0.));
#3312=DIRECTION('center_axis',(0.,0.,1.));
#3313=DIRECTION('ref_axis',(1.,0.,0.));
#3314=DIRECTION('',(0.,0.,1.));
#3315=DIRECTION('center_axis',(0.,0.,-1.));
#3316=DIRECTION('ref_axis',(1.,0.,0.));
#3317=DIRECTION('center_axis',(0.,0.,1.));
#3318=DIRECTION('ref_axis',(1.,0.,0.));
#3319=DIRECTION('center_axis',(0.,0.,1.));
#3320=DIRECTION('ref_axis',(1.,0.,0.));
#3321=DIRECTION('',(0.,0.,1.));
#3322=DIRECTION('center_axis',(0.,0.,-1.));
#3323=DIRECTION('ref_axis',(1.,0.,0.));
#3324=DIRECTION('center_axis',(0.,0.,1.));
#3325=DIRECTION('ref_axis',(1.,0.,0.));
#3326=DIRECTION('center_axis',(0.,0.,1.));
#3327=DIRECTION('ref_axis',(1.,0.,0.));
#3328=DIRECTION('',(0.,0.,1.));
#3329=DIRECTION('center_axis',(0.,0.,-1.));
#3330=DIRECTION('ref_axis',(1.,0.,0.));
#3331=DIRECTION('center_axis',(0.,0.,1.));
#3332=DIRECTION('ref_axis',(1.,0.,0.));
#3333=DIRECTION('center_axis',(0.,0.,1.));
#3334=DIRECTION('ref_axis',(1.,0.,0.));
#3335=DIRECTION('',(0.,0.,1.));
#3336=DIRECTION('center_axis',(0.,0.,-1.));
#3337=DIRECTION('ref_axis',(1.,0.,0.));
#3338=DIRECTION('center_axis',(0.,0.,1.));
#3339=DIRECTION('ref_axis',(1.,0.,0.));
#3340=DIRECTION('center_axis',(0.,0.,1.));
#3341=DIRECTION('ref_axis',(1.,0.,0.));
#3342=DIRECTION('',(0.,0.,1.));
#3343=DIRECTION('center_axis',(0.,0.,-1.));
#3344=DIRECTION('ref_axis',(1.,0.,0.));
#3345=DIRECTION('center_axis',(0.,1.,0.));
#3346=DIRECTION('ref_axis',(-1.,0.,0.));
#3347=DIRECTION('',(-1.,0.,0.));
#3348=DIRECTION('',(0.,0.,1.));
#3349=DIRECTION('',(-1.,0.,0.));
#3350=DIRECTION('',(0.,0.,1.));
#3351=DIRECTION('center_axis',(1.,0.,0.));
#3352=DIRECTION('ref_axis',(0.,1.,0.));
#3353=DIRECTION('',(0.,1.,0.));
#3354=DIRECTION('',(0.,1.,0.));
#3355=DIRECTION('',(0.,0.,1.));
#3356=DIRECTION('center_axis',(0.,-1.,0.));
#3357=DIRECTION('ref_axis',(1.,0.,0.));
#3358=DIRECTION('',(1.,0.,0.));
#3359=DIRECTION('',(1.,0.,0.));
#3360=DIRECTION('',(0.,0.,1.));
#3361=DIRECTION('center_axis',(-1.,0.,0.));
#3362=DIRECTION('ref_axis',(0.,-1.,0.));
#3363=DIRECTION('',(0.,-1.,0.));
#3364=DIRECTION('',(0.,-1.,0.));
#3365=DIRECTION('center_axis',(0.,0.,1.));
#3366=DIRECTION('ref_axis',(1.,0.,0.));
#3367=DIRECTION('center_axis',(0.,0.,1.));
#3368=DIRECTION('ref_axis',(1.,0.,0.));
#3369=DIRECTION('axis',(0.,0.,1.));
#3370=DIRECTION('refdir',(1.,0.,0.));
#3371=DIRECTION('center_axis',(0.,0.,1.));
#3372=DIRECTION('ref_axis',(1.,0.,0.));
#3373=DIRECTION('center_axis',(0.,0.,1.));
#3374=DIRECTION('ref_axis',(1.,0.,0.));
#3375=DIRECTION('',(0.,0.,-1.));
#3376=DIRECTION('center_axis',(0.,0.,1.));
#3377=DIRECTION('ref_axis',(1.,0.,0.));
#3378=DIRECTION('center_axis',(0.,0.,1.));
#3379=DIRECTION('ref_axis',(1.,0.,0.));
#3380=DIRECTION('center_axis',(0.,0.,1.));
#3381=DIRECTION('ref_axis',(1.,0.,0.));
#3382=DIRECTION('center_axis',(0.,0.,1.));
#3383=DIRECTION('ref_axis',(1.,0.,0.));
#3384=DIRECTION('center_axis',(0.,0.,1.));
#3385=DIRECTION('ref_axis',(1.,0.,0.));
#3386=DIRECTION('center_axis',(0.,0.,1.));
#3387=DIRECTION('ref_axis',(1.,0.,0.));
#3388=DIRECTION('center_axis',(0.,0.,1.));
#3389=DIRECTION('ref_axis',(1.,0.,0.));
#3390=DIRECTION('',(0.,0.,-1.));
#3391=DIRECTION('center_axis',(0.,0.,1.));
#3392=DIRECTION('ref_axis',(1.,0.,0.));
#3393=DIRECTION('center_axis',(0.,0.,1.));
#3394=DIRECTION('ref_axis',(1.,0.,0.));
#3395=DIRECTION('',(0.,0.,-1.));
#3396=DIRECTION('center_axis',(0.,0.,1.));
#3397=DIRECTION('ref_axis',(1.,0.,0.));
#3398=DIRECTION('center_axis',(0.,0.,1.));
#3399=DIRECTION('ref_axis',(1.,0.,0.));
#3400=DIRECTION('axis',(0.,0.,1.));
#3401=DIRECTION('refdir',(1.,0.,0.));
#3402=DIRECTION('center_axis',(0.,0.,1.));
#3403=DIRECTION('ref_axis',(1.,0.,0.));
#3404=DIRECTION('center_axis',(0.,0.,-1.));
#3405=DIRECTION('ref_axis',(1.,0.,0.));
#3406=DIRECTION('',(0.,0.,-1.));
#3407=DIRECTION('center_axis',(0.,0.,-1.));
#3408=DIRECTION('ref_axis',(1.,0.,0.));
#3409=DIRECTION('center_axis',(0.,0.,1.));
#3410=DIRECTION('ref_axis',(1.,0.,0.));
#3411=DIRECTION('center_axis',(0.,0.,1.));
#3412=DIRECTION('ref_axis',(1.,0.,0.));
#3413=DIRECTION('',(0.,0.,-1.));
#3414=DIRECTION('center_axis',(0.,0.,1.));
#3415=DIRECTION('ref_axis',(1.,0.,0.));
#3416=DIRECTION('center_axis',(0.,0.,1.));
#3417=DIRECTION('ref_axis',(1.,0.,0.));
#3418=DIRECTION('center_axis',(0.,0.,1.));
#3419=DIRECTION('ref_axis',(1.,0.,0.));
#3420=DIRECTION('axis',(0.,0.,1.));
#3421=DIRECTION('refdir',(1.,0.,0.));
#3422=DIRECTION('center_axis',(0.,1.,0.));
#3423=DIRECTION('ref_axis',(1.,0.,0.));
#3424=DIRECTION('center_axis',(0.,-1.,0.));
#3425=DIRECTION('ref_axis',(1.,0.,0.));
#3426=DIRECTION('',(0.,-1.,0.));
#3427=DIRECTION('center_axis',(0.,-1.,0.));
#3428=DIRECTION('ref_axis',(1.,0.,0.));
#3429=DIRECTION('center_axis',(0.,1.,0.));
#3430=DIRECTION('ref_axis',(1.,0.,0.));
#3431=DIRECTION('center_axis',(0.,1.,0.));
#3432=DIRECTION('ref_axis',(1.,0.,0.));
#3433=DIRECTION('',(0.,-1.,0.));
#3434=DIRECTION('center_axis',(0.,1.,0.));
#3435=DIRECTION('ref_axis',(1.,0.,0.));
#3436=DIRECTION('center_axis',(0.,1.,0.));
#3437=DIRECTION('ref_axis',(1.,0.,0.));
#3438=DIRECTION('center_axis',(0.,1.,0.));
#3439=DIRECTION('ref_axis',(1.,0.,0.));
#3440=DIRECTION('axis',(0.,0.,1.));
#3441=DIRECTION('refdir',(1.,0.,0.));
#3442=DIRECTION('center_axis',(0.,1.,0.));
#3443=DIRECTION('ref_axis',(1.,0.,0.));
#3444=DIRECTION('',(0.866025403784439,-0.5,1.06057523872491E-16));
#3445=DIRECTION('center_axis',(0.,-1.,0.));
#3446=DIRECTION('ref_axis',(1.,0.,0.));
#3447=DIRECTION('center_axis',(0.,-1.,0.));
#3448=DIRECTION('ref_axis',(1.,0.,0.));
#3449=DIRECTION('center_axis',(0.,1.,0.));
#3450=DIRECTION('ref_axis',(1.,0.,0.));
#3451=DIRECTION('',(-0.866025403784439,-0.5,-1.06057523872491E-16));
#3452=DIRECTION('center_axis',(1.4792020664489E-16,0.,-1.));
#3453=DIRECTION('ref_axis',(-1.,0.,-1.4792020664489E-16));
#3454=DIRECTION('',(0.,1.,0.));
#3455=DIRECTION('',(0.,1.,0.));
#3456=DIRECTION('center_axis',(-0.866025403784439,0.,-0.5));
#3457=DIRECTION('ref_axis',(-0.5,0.,0.866025403784439));
#3458=DIRECTION('',(0.,1.,0.));
#3459=DIRECTION('center_axis',(-0.866025403784439,0.,0.5));
#3460=DIRECTION('ref_axis',(0.5,0.,0.866025403784439));
#3461=DIRECTION('',(0.,1.,0.));
#3462=DIRECTION('center_axis',(0.,1.,0.));
#3463=DIRECTION('ref_axis',(1.,0.,0.));
#3464=DIRECTION('center_axis',(0.,1.,0.));
#3465=DIRECTION('ref_axis',(1.,0.,0.));
#3466=DIRECTION('',(0.,-1.,0.));
#3467=DIRECTION('center_axis',(0.,1.,0.));
#3468=DIRECTION('ref_axis',(1.,0.,0.));
#3469=DIRECTION('center_axis',(-2.95840413289779E-16,0.,1.));
#3470=DIRECTION('ref_axis',(1.,0.,2.95840413289779E-16));
#3471=DIRECTION('',(0.,1.,0.));
#3472=DIRECTION('center_axis',(0.866025403784439,0.,-0.5));
#3473=DIRECTION('ref_axis',(-0.5,0.,-0.866025403784439));
#3474=DIRECTION('',(0.,1.,0.));
#3475=DIRECTION('center_axis',(0.866025403784439,0.,0.5));
#3476=DIRECTION('ref_axis',(0.5,0.,-0.866025403784439));
#3477=DIRECTION('center_axis',(0.,1.,0.));
#3478=DIRECTION('ref_axis',(1.,0.,0.));
#3479=DIRECTION('center_axis',(0.,1.,0.));
#3480=DIRECTION('ref_axis',(1.,0.,0.));
#3481=DIRECTION('',(0.,0.,1.));
#3482=DIRECTION('',(1.,0.,0.));
#3483=DIRECTION('',(0.,0.,1.));
#3484=DIRECTION('',(1.,0.,0.));
#3485=DIRECTION('',(0.,0.,1.));
#3486=DIRECTION('',(1.,0.,0.));
#3487=DIRECTION('',(0.,1.,2.22044604925031E-16));
#3488=DIRECTION('',(1.,0.,0.));
#3489=DIRECTION('',(0.,1.,2.22044604925031E-16));
#3490=DIRECTION('',(1.,0.,0.));
#3491=DIRECTION('axis',(0.,0.,1.));
#3492=DIRECTION('refdir',(1.,0.,0.));
#3493=DIRECTION('axis',(0.,0.,1.));
#3494=DIRECTION('refdir',(1.,0.,0.));
#3495=DIRECTION('center_axis',(0.,0.,1.));
#3496=DIRECTION('ref_axis',(1.,0.,0.));
#3497=DIRECTION('center_axis',(0.,0.,1.));
#3498=DIRECTION('ref_axis',(1.,0.,0.));
#3499=DIRECTION('',(0.,0.,1.));
#3500=DIRECTION('center_axis',(0.,0.,-1.));
#3501=DIRECTION('ref_axis',(1.,0.,0.));
#3502=DIRECTION('center_axis',(0.,1.,0.));
#3503=DIRECTION('ref_axis',(1.,0.,0.));
#3504=DIRECTION('center_axis',(0.,-1.,0.));
#3505=DIRECTION('ref_axis',(1.,0.,0.));
#3506=DIRECTION('',(0.,1.,0.));
#3507=DIRECTION('center_axis',(0.,1.,0.));
#3508=DIRECTION('ref_axis',(1.,0.,0.));
#3509=DIRECTION('',(0.,-1.,0.));
#3510=DIRECTION('center_axis',(0.,1.,0.));
#3511=DIRECTION('ref_axis',(1.,0.,0.));
#3512=DIRECTION('',(0.,-1.,0.));
#3513=DIRECTION('center_axis',(0.,-1.,0.));
#3514=DIRECTION('ref_axis',(1.,0.,0.));
#3515=DIRECTION('',(0.,1.,0.));
#3516=DIRECTION('center_axis',(0.,1.,0.));
#3517=DIRECTION('ref_axis',(1.,0.,0.));
#3518=DIRECTION('center_axis',(0.,1.,0.));
#3519=DIRECTION('ref_axis',(-1.,0.,0.));
#3520=DIRECTION('',(-1.,0.,0.));
#3521=DIRECTION('',(0.,0.,1.));
#3522=DIRECTION('',(-1.,0.,0.));
#3523=DIRECTION('',(0.,0.,1.));
#3524=DIRECTION('',(-1.,0.,0.));
#3525=DIRECTION('',(0.,0.,1.));
#3526=DIRECTION('',(-1.,0.,0.));
#3527=DIRECTION('center_axis',(0.,0.,-1.));
#3528=DIRECTION('ref_axis',(-1.,0.,0.));
#3529=DIRECTION('',(1.,0.,0.));
#3530=DIRECTION('',(0.,1.,0.));
#3531=DIRECTION('center_axis',(0.,0.,-1.));
#3532=DIRECTION('ref_axis',(-1.,0.,0.));
#3533=DIRECTION('',(0.,1.,0.));
#3534=DIRECTION('',(1.,0.,0.));
#3535=DIRECTION('center_axis',(0.,-1.,0.));
#3536=DIRECTION('ref_axis',(1.,0.,0.));
#3537=DIRECTION('',(1.,0.,0.));
#3538=DIRECTION('',(0.,0.,1.));
#3539=DIRECTION('',(1.,0.,0.));
#3540=DIRECTION('',(0.,0.,1.));
#3541=DIRECTION('',(1.,0.,0.));
#3542=DIRECTION('',(0.,0.,-1.));
#3543=DIRECTION('',(1.,0.,0.));
#3544=DIRECTION('center_axis',(0.,0.,-1.));
#3545=DIRECTION('ref_axis',(-1.,0.,0.));
#3546=DIRECTION('',(-1.,0.,0.));
#3547=DIRECTION('',(0.,1.,0.));
#3548=DIRECTION('center_axis',(-1.,0.,0.));
#3549=DIRECTION('ref_axis',(0.,0.,1.));
#3550=DIRECTION('',(0.,-1.,0.));
#3551=DIRECTION('',(0.,0.,-1.));
#3552=DIRECTION('center_axis',(0.,1.,0.));
#3553=DIRECTION('ref_axis',(1.,0.,0.));
#3554=DIRECTION('',(0.,0.,1.));
#3555=DIRECTION('',(1.,0.,0.));
#3556=DIRECTION('center_axis',(0.,0.,1.));
#3557=DIRECTION('ref_axis',(1.,0.,0.));
#3558=DIRECTION('',(0.,1.,0.));
#3559=DIRECTION('',(-1.,0.,0.));
#3560=DIRECTION('',(0.,-1.,0.));
#3561=DIRECTION('',(0.,-1.,0.));
#3562=DIRECTION('center_axis',(1.,0.,0.));
#3563=DIRECTION('ref_axis',(0.,1.,0.));
#3564=DIRECTION('',(0.,1.,0.));
#3565=DIRECTION('',(0.,0.,-1.));
#3566=DIRECTION('center_axis',(0.,1.,0.));
#3567=DIRECTION('ref_axis',(0.,0.,1.));
#3568=DIRECTION('',(-1.,0.,0.));
#3569=DIRECTION('',(0.,0.,1.));
#3570=DIRECTION('center_axis',(-1.,0.,0.));
#3571=DIRECTION('ref_axis',(0.,0.,1.));
#3572=DIRECTION('',(0.,1.,0.));
#3573=DIRECTION('center_axis',(0.,0.,-1.));
#3574=DIRECTION('ref_axis',(-1.,0.,0.));
#3575=DIRECTION('center_axis',(-1.,0.,0.));
#3576=DIRECTION('ref_axis',(0.,-1.,0.));
#3577=DIRECTION('',(0.,-1.,0.));
#3578=DIRECTION('center_axis',(0.,0.,1.));
#3579=DIRECTION('ref_axis',(1.,0.,0.));
#3580=DIRECTION('axis',(0.,0.,1.));
#3581=DIRECTION('refdir',(1.,0.,0.));
#3582=DIRECTION('center_axis',(0.,0.,1.));
#3583=DIRECTION('ref_axis',(1.,0.,0.));
#3584=DIRECTION('center_axis',(0.,0.,-1.));
#3585=DIRECTION('ref_axis',(1.,0.,0.));
#3586=DIRECTION('',(0.,0.,-1.));
#3587=DIRECTION('center_axis',(0.,0.,-1.));
#3588=DIRECTION('ref_axis',(1.,0.,0.));
#3589=DIRECTION('center_axis',(0.,0.,1.));
#3590=DIRECTION('ref_axis',(1.,0.,0.));
#3591=DIRECTION('center_axis',(0.,0.,1.));
#3592=DIRECTION('ref_axis',(1.,0.,0.));
#3593=DIRECTION('',(0.,0.,-1.));
#3594=DIRECTION('center_axis',(0.,0.,1.));
#3595=DIRECTION('ref_axis',(1.,0.,0.));
#3596=DIRECTION('center_axis',(0.,0.,1.));
#3597=DIRECTION('ref_axis',(1.,0.,0.));
#3598=DIRECTION('center_axis',(0.,0.,1.));
#3599=DIRECTION('ref_axis',(1.,0.,0.));
#3600=DIRECTION('axis',(0.,0.,1.));
#3601=DIRECTION('refdir',(1.,0.,0.));
#3602=DIRECTION('center_axis',(0.,0.,1.));
#3603=DIRECTION('ref_axis',(1.,0.,0.));
#3604=DIRECTION('center_axis',(0.,0.,-1.));
#3605=DIRECTION('ref_axis',(1.,0.,0.));
#3606=DIRECTION('',(0.,0.,-1.));
#3607=DIRECTION('center_axis',(0.,0.,-1.));
#3608=DIRECTION('ref_axis',(1.,0.,0.));
#3609=DIRECTION('center_axis',(0.,0.,1.));
#3610=DIRECTION('ref_axis',(1.,0.,0.));
#3611=DIRECTION('center_axis',(0.,0.,1.));
#3612=DIRECTION('ref_axis',(1.,0.,0.));
#3613=DIRECTION('',(0.,0.,-1.));
#3614=DIRECTION('center_axis',(0.,0.,1.));
#3615=DIRECTION('ref_axis',(1.,0.,0.));
#3616=DIRECTION('center_axis',(0.,0.,1.));
#3617=DIRECTION('ref_axis',(1.,0.,0.));
#3618=DIRECTION('center_axis',(0.,0.,1.));
#3619=DIRECTION('ref_axis',(1.,0.,0.));
#3620=DIRECTION('axis',(0.,0.,1.));
#3621=DIRECTION('refdir',(1.,0.,0.));
#3622=DIRECTION('center_axis',(0.,0.,1.));
#3623=DIRECTION('ref_axis',(1.,0.,0.));
#3624=DIRECTION('center_axis',(0.,0.,-1.));
#3625=DIRECTION('ref_axis',(1.,0.,0.));
#3626=DIRECTION('',(0.,0.,-1.));
#3627=DIRECTION('center_axis',(0.,0.,-1.));
#3628=DIRECTION('ref_axis',(1.,0.,0.));
#3629=DIRECTION('center_axis',(0.,0.,1.));
#3630=DIRECTION('ref_axis',(1.,0.,0.));
#3631=DIRECTION('center_axis',(0.,0.,1.));
#3632=DIRECTION('ref_axis',(1.,0.,0.));
#3633=DIRECTION('',(0.,0.,-1.));
#3634=DIRECTION('center_axis',(0.,0.,1.));
#3635=DIRECTION('ref_axis',(1.,0.,0.));
#3636=DIRECTION('center_axis',(0.,0.,1.));
#3637=DIRECTION('ref_axis',(1.,0.,0.));
#3638=DIRECTION('center_axis',(0.,0.,1.));
#3639=DIRECTION('ref_axis',(1.,0.,0.));
#3640=DIRECTION('axis',(0.,0.,1.));
#3641=DIRECTION('refdir',(1.,0.,0.));
#3642=DIRECTION('center_axis',(0.,1.,0.));
#3643=DIRECTION('ref_axis',(1.,0.,0.));
#3644=DIRECTION('center_axis',(0.,1.,0.));
#3645=DIRECTION('ref_axis',(1.,0.,0.));
#3646=DIRECTION('',(0.,1.,0.));
#3647=DIRECTION('center_axis',(0.,-1.,0.));
#3648=DIRECTION('ref_axis',(1.,0.,0.));
#3649=DIRECTION('center_axis',(0.,1.,0.));
#3650=DIRECTION('ref_axis',(1.,0.,0.));
#3651=DIRECTION('center_axis',(0.,1.,0.));
#3652=DIRECTION('ref_axis',(1.,0.,0.));
#3653=DIRECTION('center_axis',(0.,1.,0.));
#3654=DIRECTION('ref_axis',(1.,0.,0.));
#3655=DIRECTION('center_axis',(0.,1.,0.));
#3656=DIRECTION('ref_axis',(1.,0.,0.));
#3657=DIRECTION('center_axis',(0.,1.,0.));
#3658=DIRECTION('ref_axis',(1.,0.,0.));
#3659=DIRECTION('',(0.,-1.,0.));
#3660=DIRECTION('center_axis',(0.,1.,0.));
#3661=DIRECTION('ref_axis',(1.,0.,0.));
#3662=DIRECTION('center_axis',(0.,1.,0.));
#3663=DIRECTION('ref_axis',(1.,0.,0.));
#3664=DIRECTION('center_axis',(0.,1.,0.));
#3665=DIRECTION('ref_axis',(1.,0.,0.));
#3666=DIRECTION('center_axis',(0.,1.,0.));
#3667=DIRECTION('ref_axis',(1.,0.,0.));
#3668=DIRECTION('',(0.,-1.,0.));
#3669=DIRECTION('center_axis',(0.,1.,0.));
#3670=DIRECTION('ref_axis',(1.,0.,0.));
#3671=DIRECTION('axis',(0.,0.,1.));
#3672=DIRECTION('refdir',(1.,0.,0.));
#3673=DIRECTION('center_axis',(0.,1.,0.));
#3674=DIRECTION('ref_axis',(1.,0.,0.));
#3675=DIRECTION('center_axis',(0.,-1.,0.));
#3676=DIRECTION('ref_axis',(1.,0.,0.));
#3677=DIRECTION('',(0.,-1.,0.));
#3678=DIRECTION('center_axis',(0.,-1.,0.));
#3679=DIRECTION('ref_axis',(1.,0.,0.));
#3680=DIRECTION('center_axis',(0.,1.,0.));
#3681=DIRECTION('ref_axis',(1.,0.,0.));
#3682=DIRECTION('center_axis',(0.,1.,0.));
#3683=DIRECTION('ref_axis',(1.,0.,0.));
#3684=DIRECTION('',(0.,-1.,0.));
#3685=DIRECTION('center_axis',(0.,1.,0.));
#3686=DIRECTION('ref_axis',(1.,0.,0.));
#3687=DIRECTION('center_axis',(0.,1.,0.));
#3688=DIRECTION('ref_axis',(1.,0.,0.));
#3689=DIRECTION('center_axis',(0.,1.,0.));
#3690=DIRECTION('ref_axis',(1.,0.,0.));
#3691=DIRECTION('axis',(0.,0.,1.));
#3692=DIRECTION('refdir',(1.,0.,0.));
#3693=DIRECTION('center_axis',(0.,1.,0.));
#3694=DIRECTION('ref_axis',(1.,0.,0.));
#3695=DIRECTION('center_axis',(0.,-1.,0.));
#3696=DIRECTION('ref_axis',(1.,0.,0.));
#3697=DIRECTION('',(0.,-1.,0.));
#3698=DIRECTION('center_axis',(0.,-1.,0.));
#3699=DIRECTION('ref_axis',(1.,0.,0.));
#3700=DIRECTION('center_axis',(0.,1.,0.));
#3701=DIRECTION('ref_axis',(1.,0.,0.));
#3702=DIRECTION('center_axis',(0.,1.,0.));
#3703=DIRECTION('ref_axis',(1.,0.,0.));
#3704=DIRECTION('',(0.,-1.,0.));
#3705=DIRECTION('center_axis',(0.,1.,0.));
#3706=DIRECTION('ref_axis',(1.,0.,0.));
#3707=DIRECTION('center_axis',(0.,1.,0.));
#3708=DIRECTION('ref_axis',(1.,0.,0.));
#3709=DIRECTION('center_axis',(0.,1.,0.));
#3710=DIRECTION('ref_axis',(1.,0.,0.));
#3711=DIRECTION('axis',(0.,0.,1.));
#3712=DIRECTION('refdir',(1.,0.,0.));
#3713=DIRECTION('center_axis',(0.,1.,0.));
#3714=DIRECTION('ref_axis',(1.,0.,0.));
#3715=DIRECTION('center_axis',(0.,-1.,0.));
#3716=DIRECTION('ref_axis',(1.,0.,0.));
#3717=DIRECTION('',(0.,-1.,0.));
#3718=DIRECTION('center_axis',(0.,-1.,0.));
#3719=DIRECTION('ref_axis',(1.,0.,0.));
#3720=DIRECTION('center_axis',(0.,1.,0.));
#3721=DIRECTION('ref_axis',(1.,0.,0.));
#3722=DIRECTION('center_axis',(0.,1.,0.));
#3723=DIRECTION('ref_axis',(1.,0.,0.));
#3724=DIRECTION('',(0.,-1.,0.));
#3725=DIRECTION('center_axis',(0.,1.,0.));
#3726=DIRECTION('ref_axis',(1.,0.,0.));
#3727=DIRECTION('center_axis',(0.,1.,0.));
#3728=DIRECTION('ref_axis',(1.,0.,0.));
#3729=DIRECTION('center_axis',(0.,1.,0.));
#3730=DIRECTION('ref_axis',(1.,0.,0.));
#3731=DIRECTION('axis',(0.,0.,1.));
#3732=DIRECTION('refdir',(1.,0.,0.));
#3733=DIRECTION('center_axis',(0.866025403784439,0.,-0.5));
#3734=DIRECTION('ref_axis',(0.5,0.,0.866025403784439));
#3735=DIRECTION('',(-0.5,0.,-0.866025403784439));
#3736=DIRECTION('',(0.,-1.,0.));
#3737=DIRECTION('',(0.5,0.,0.866025403784439));
#3738=DIRECTION('',(0.,-1.,0.));
#3739=DIRECTION('center_axis',(1.60246890531964E-16,0.,-1.));
#3740=DIRECTION('ref_axis',(1.,0.,1.60246890531964E-16));
#3741=DIRECTION('',(-1.,0.,-1.60246890531964E-16));
#3742=DIRECTION('',(0.,-1.,0.));
#3743=DIRECTION('',(1.,0.,1.60246890531964E-16));
#3744=DIRECTION('center_axis',(-0.866025403784439,0.,-0.5));
#3745=DIRECTION('ref_axis',(0.5,0.,-0.866025403784439));
#3746=DIRECTION('',(-0.5,0.,0.866025403784439));
#3747=DIRECTION('',(0.,-1.,0.));
#3748=DIRECTION('',(0.5,0.,-0.866025403784439));
#3749=DIRECTION('center_axis',(-0.866025403784439,0.,0.5));
#3750=DIRECTION('ref_axis',(-0.5,0.,-0.866025403784439));
#3751=DIRECTION('',(0.5,0.,0.866025403784439));
#3752=DIRECTION('',(0.,-1.,0.));
#3753=DIRECTION('',(-0.5,0.,-0.866025403784439));
#3754=DIRECTION('center_axis',(-1.60246890531964E-16,0.,1.));
#3755=DIRECTION('ref_axis',(-1.,0.,-1.60246890531964E-16));
#3756=DIRECTION('',(1.,0.,1.60246890531964E-16));
#3757=DIRECTION('',(0.,-1.,0.));
#3758=DIRECTION('',(-1.,0.,-1.60246890531964E-16));
#3759=DIRECTION('center_axis',(0.866025403784439,0.,0.5));
#3760=DIRECTION('ref_axis',(-0.5,0.,0.866025403784439));
#3761=DIRECTION('',(0.5,0.,-0.866025403784439));
#3762=DIRECTION('',(-0.5,0.,0.866025403784439));
#3763=DIRECTION('center_axis',(0.,1.,0.));
#3764=DIRECTION('ref_axis',(1.,0.,0.));
#3765=DIRECTION('center_axis',(0.,-1.,0.));
#3766=DIRECTION('ref_axis',(0.,0.,-1.));
#3767=DIRECTION('center_axis',(0.,1.,0.));
#3768=DIRECTION('ref_axis',(1.,0.,0.));
#3769=DIRECTION('center_axis',(0.,1.,0.));
#3770=DIRECTION('ref_axis',(1.,0.,0.));
#3771=DIRECTION('center_axis',(0.,1.,0.));
#3772=DIRECTION('ref_axis',(0.,0.,1.));
#3773=DIRECTION('center_axis',(0.,-1.,0.));
#3774=DIRECTION('ref_axis',(1.,0.,0.));
#3775=DIRECTION('center_axis',(0.,-1.,0.));
#3776=DIRECTION('ref_axis',(1.,0.,0.));
#3777=DIRECTION('center_axis',(0.,-1.,0.));
#3778=DIRECTION('ref_axis',(1.,0.,0.));
#3779=DIRECTION('',(0.707106781186547,0.707106781186548,8.65956056235493E-17));
#3780=DIRECTION('center_axis',(0.,-1.,0.));
#3781=DIRECTION('ref_axis',(1.,0.,0.));
#3782=DIRECTION('center_axis',(0.,-1.,0.));
#3783=DIRECTION('ref_axis',(1.,0.,0.));
#3784=DIRECTION('',(0.,1.,0.));
#3785=DIRECTION('center_axis',(0.,1.,0.));
#3786=DIRECTION('ref_axis',(1.,0.,0.));
#3787=DIRECTION('center_axis',(0.,-1.,0.));
#3788=DIRECTION('ref_axis',(1.,0.,0.));
#3789=DIRECTION('',(-0.707106781186547,0.707106781186548,-8.65956056235493E-17));
#3790=DIRECTION('center_axis',(0.,-1.,0.));
#3791=DIRECTION('ref_axis',(0.,0.,-1.));
#3792=DIRECTION('center_axis',(0.,-1.,0.));
#3793=DIRECTION('ref_axis',(1.,0.,0.));
#3794=DIRECTION('center_axis',(0.,1.,0.));
#3795=DIRECTION('ref_axis',(1.,0.,0.));
#3796=DIRECTION('center_axis',(0.,1.,0.));
#3797=DIRECTION('ref_axis',(1.,0.,0.));
#3798=DIRECTION('',(-0.447213595499958,0.894427190999916,-5.47678698264203E-17));
#3799=DIRECTION('center_axis',(0.,-1.,0.));
#3800=DIRECTION('ref_axis',(1.,0.,0.));
#3801=DIRECTION('',(0.,1.,0.));
#3802=DIRECTION('',(0.,0.,1.));
#3803=DIRECTION('',(1.,0.,0.));
#3804=DIRECTION('',(0.,0.,1.));
#3805=DIRECTION('',(1.,0.,0.));
#3806=DIRECTION('',(0.,0.,1.));
#3807=DIRECTION('',(1.,0.,0.));
#3808=DIRECTION('',(0.,0.,1.));
#3809=DIRECTION('',(1.,0.,0.));
#3810=DIRECTION('',(0.,0.,1.));
#3811=DIRECTION('',(1.,0.,0.));
#3812=DIRECTION('',(0.,0.,1.));
#3813=DIRECTION('',(1.,0.,0.));
#3814=DIRECTION('',(0.,0.,1.));
#3815=DIRECTION('',(1.,0.,0.));
#3816=DIRECTION('',(0.,0.,1.));
#3817=DIRECTION('',(1.,0.,0.));
#3818=DIRECTION('',(0.,0.,1.));
#3819=DIRECTION('',(1.,0.,0.));
#3820=DIRECTION('axis',(0.,0.,1.));
#3821=DIRECTION('refdir',(1.,0.,0.));
#3822=DIRECTION('axis',(0.,0.,1.));
#3823=DIRECTION('refdir',(1.,0.,0.));
#3824=DIRECTION('center_axis',(0.,1.,0.));
#3825=DIRECTION('ref_axis',(1.,0.,0.));
#3826=DIRECTION('center_axis',(0.,1.,0.));
#3827=DIRECTION('ref_axis',(1.,0.,0.));
#3828=DIRECTION('',(0.,1.,0.));
#3829=DIRECTION('center_axis',(0.,-1.,0.));
#3830=DIRECTION('ref_axis',(1.,0.,0.));
#3831=DIRECTION('center_axis',(0.,1.,0.));
#3832=DIRECTION('ref_axis',(1.,0.,0.));
#3833=DIRECTION('center_axis',(0.,1.,0.));
#3834=DIRECTION('ref_axis',(1.,0.,0.));
#3835=DIRECTION('center_axis',(0.,1.,0.));
#3836=DIRECTION('ref_axis',(1.,0.,0.));
#3837=DIRECTION('center_axis',(0.,1.,0.));
#3838=DIRECTION('ref_axis',(1.,0.,0.));
#3839=DIRECTION('',(0.,1.,0.));
#3840=DIRECTION('center_axis',(0.,1.,0.));
#3841=DIRECTION('ref_axis',(1.,0.,0.));
#3842=DIRECTION('center_axis',(0.,1.,0.));
#3843=DIRECTION('ref_axis',(1.,0.,0.));
#3844=DIRECTION('center_axis',(0.,-1.,0.));
#3845=DIRECTION('ref_axis',(1.,0.,0.));
#3846=DIRECTION('center_axis',(0.,1.,0.));
#3847=DIRECTION('ref_axis',(1.,0.,0.));
#3848=DIRECTION('',(0.,-1.,0.));
#3849=DIRECTION('center_axis',(0.,1.,0.));
#3850=DIRECTION('ref_axis',(1.,0.,0.));
#3851=DIRECTION('center_axis',(0.,1.,0.));
#3852=DIRECTION('ref_axis',(1.,0.,0.));
#3853=DIRECTION('',(0.,-1.,0.));
#3854=DIRECTION('center_axis',(0.,1.,0.));
#3855=DIRECTION('ref_axis',(1.,0.,0.));
#3856=DIRECTION('center_axis',(0.,1.,0.));
#3857=DIRECTION('ref_axis',(1.,0.,0.));
#3858=DIRECTION('center_axis',(0.,1.,0.));
#3859=DIRECTION('ref_axis',(1.,0.,0.));
#3860=DIRECTION('axis',(0.,0.,1.));
#3861=DIRECTION('refdir',(1.,0.,0.));
#3862=DIRECTION('center_axis',(0.,1.,0.));
#3863=DIRECTION('ref_axis',(1.,0.,0.));
#3864=DIRECTION('center_axis',(0.,-1.,0.));
#3865=DIRECTION('ref_axis',(1.,0.,0.));
#3866=DIRECTION('',(0.,-1.,0.));
#3867=DIRECTION('center_axis',(0.,-1.,0.));
#3868=DIRECTION('ref_axis',(1.,0.,0.));
#3869=DIRECTION('center_axis',(0.,1.,0.));
#3870=DIRECTION('ref_axis',(1.,0.,0.));
#3871=DIRECTION('center_axis',(0.,1.,0.));
#3872=DIRECTION('ref_axis',(1.,0.,0.));
#3873=DIRECTION('',(0.,-1.,0.));
#3874=DIRECTION('center_axis',(0.,1.,0.));
#3875=DIRECTION('ref_axis',(1.,0.,0.));
#3876=DIRECTION('center_axis',(0.,1.,0.));
#3877=DIRECTION('ref_axis',(1.,0.,0.));
#3878=DIRECTION('center_axis',(0.,1.,0.));
#3879=DIRECTION('ref_axis',(1.,0.,0.));
#3880=DIRECTION('axis',(0.,0.,1.));
#3881=DIRECTION('refdir',(1.,0.,0.));
#3882=DIRECTION('center_axis',(0.,1.,0.));
#3883=DIRECTION('ref_axis',(1.,0.,0.));
#3884=DIRECTION('center_axis',(0.,-1.,0.));
#3885=DIRECTION('ref_axis',(1.,0.,0.));
#3886=DIRECTION('',(0.,-1.,0.));
#3887=DIRECTION('center_axis',(0.,-1.,0.));
#3888=DIRECTION('ref_axis',(1.,0.,0.));
#3889=DIRECTION('center_axis',(0.,1.,0.));
#3890=DIRECTION('ref_axis',(1.,0.,0.));
#3891=DIRECTION('center_axis',(0.,1.,0.));
#3892=DIRECTION('ref_axis',(1.,0.,0.));
#3893=DIRECTION('',(0.,-1.,0.));
#3894=DIRECTION('center_axis',(0.,1.,0.));
#3895=DIRECTION('ref_axis',(1.,0.,0.));
#3896=DIRECTION('center_axis',(0.,1.,0.));
#3897=DIRECTION('ref_axis',(1.,0.,0.));
#3898=DIRECTION('center_axis',(0.,1.,0.));
#3899=DIRECTION('ref_axis',(1.,0.,0.));
#3900=DIRECTION('axis',(0.,0.,1.));
#3901=DIRECTION('refdir',(1.,0.,0.));
#3902=DIRECTION('axis',(0.,0.,1.));
#3903=DIRECTION('refdir',(1.,0.,0.));
#3904=DIRECTION('center_axis',(0.,-1.,0.));
#3905=DIRECTION('ref_axis',(0.,0.,-1.));
#3906=DIRECTION('center_axis',(0.,-1.,0.));
#3907=DIRECTION('ref_axis',(1.,0.,0.));
#3908=DIRECTION('center_axis',(0.,-1.,0.));
#3909=DIRECTION('ref_axis',(1.,0.,0.));
#3910=DIRECTION('center_axis',(1.,0.,1.22464679914735E-16));
#3911=DIRECTION('ref_axis',(-1.22464679914735E-16,0.,1.));
#3912=DIRECTION('center_axis',(0.,1.,0.));
#3913=DIRECTION('ref_axis',(1.,0.,0.));
#3914=DIRECTION('center_axis',(0.,1.,0.));
#3915=DIRECTION('ref_axis',(1.,0.,0.));
#3916=DIRECTION('center_axis',(0.,-1.,0.));
#3917=DIRECTION('ref_axis',(1.,0.,0.));
#3918=DIRECTION('',(0.,1.,0.));
#3919=DIRECTION('center_axis',(0.,-1.,0.));
#3920=DIRECTION('ref_axis',(1.,0.,0.));
#3921=DIRECTION('center_axis',(0.,-1.,0.));
#3922=DIRECTION('ref_axis',(1.,0.,0.));
#3923=DIRECTION('center_axis',(0.,-1.,0.));
#3924=DIRECTION('ref_axis',(1.,0.,0.));
#3925=DIRECTION('',(0.,1.,0.));
#3926=DIRECTION('center_axis',(0.,-1.,0.));
#3927=DIRECTION('ref_axis',(1.,0.,0.));
#3928=DIRECTION('center_axis',(0.,1.,0.));
#3929=DIRECTION('ref_axis',(1.,0.,0.));
#3930=DIRECTION('',(-0.707106781186547,0.707106781186548,-8.65956056235493E-17));
#3931=DIRECTION('center_axis',(0.,-1.,0.));
#3932=DIRECTION('ref_axis',(1.,0.,0.));
#3933=DIRECTION('center_axis',(0.,1.,0.));
#3934=DIRECTION('ref_axis',(0.,0.,1.));
#3935=DIRECTION('center_axis',(0.,-1.,0.));
#3936=DIRECTION('ref_axis',(1.,0.,0.));
#3937=DIRECTION('center_axis',(0.,-1.,0.));
#3938=DIRECTION('ref_axis',(1.,0.,0.));
#3939=DIRECTION('',(0.,1.,0.));
#3940=DIRECTION('center_axis',(0.,-1.,0.));
#3941=DIRECTION('ref_axis',(0.,0.,-1.));
#3942=DIRECTION('center_axis',(0.,-1.,0.));
#3943=DIRECTION('ref_axis',(1.,0.,0.));
#3944=DIRECTION('center_axis',(0.,-1.,0.));
#3945=DIRECTION('ref_axis',(1.,0.,0.));
#3946=DIRECTION('',(0.707106781186547,0.707106781186548,8.65956056235493E-17));
#3947=DIRECTION('axis',(0.,0.,1.));
#3948=DIRECTION('refdir',(1.,0.,0.));
#3949=DIRECTION('center_axis',(0.,-1.,0.));
#3950=DIRECTION('ref_axis',(0.,0.,-1.));
#3951=DIRECTION('center_axis',(0.,-1.,0.));
#3952=DIRECTION('ref_axis',(1.,0.,0.));
#3953=DIRECTION('center_axis',(0.,-1.,0.));
#3954=DIRECTION('ref_axis',(1.,0.,0.));
#3955=DIRECTION('center_axis',(1.,0.,1.22464679914735E-16));
#3956=DIRECTION('ref_axis',(-1.22464679914735E-16,0.,1.));
#3957=DIRECTION('center_axis',(0.,1.,0.));
#3958=DIRECTION('ref_axis',(1.,0.,0.));
#3959=DIRECTION('center_axis',(0.,1.,0.));
#3960=DIRECTION('ref_axis',(1.,0.,0.));
#3961=DIRECTION('center_axis',(0.,-1.,0.));
#3962=DIRECTION('ref_axis',(1.,0.,0.));
#3963=DIRECTION('center_axis',(0.,-1.,0.));
#3964=DIRECTION('ref_axis',(1.,0.,0.));
#3965=DIRECTION('',(0.,1.,0.));
#3966=DIRECTION('center_axis',(0.,1.,0.));
#3967=DIRECTION('ref_axis',(0.,0.,1.));
#3968=DIRECTION('center_axis',(0.,-1.,0.));
#3969=DIRECTION('ref_axis',(1.,0.,0.));
#3970=DIRECTION('center_axis',(0.,-1.,0.));
#3971=DIRECTION('ref_axis',(1.,0.,0.));
#3972=DIRECTION('center_axis',(0.,-1.,0.));
#3973=DIRECTION('ref_axis',(1.,0.,0.));
#3974=DIRECTION('center_axis',(0.,-1.,0.));
#3975=DIRECTION('ref_axis',(1.,0.,0.));
#3976=DIRECTION('',(0.707106781186548,0.707106781186547,8.65956056235494E-17));
#3977=DIRECTION('center_axis',(0.,-1.,0.));
#3978=DIRECTION('ref_axis',(1.,0.,0.));
#3979=DIRECTION('center_axis',(0.,-1.,0.));
#3980=DIRECTION('ref_axis',(1.,0.,0.));
#3981=DIRECTION('',(0.,1.,0.));
#3982=DIRECTION('center_axis',(0.,1.,0.));
#3983=DIRECTION('ref_axis',(1.,0.,0.));
#3984=DIRECTION('center_axis',(0.,-1.,0.));
#3985=DIRECTION('ref_axis',(1.,0.,0.));
#3986=DIRECTION('',(-0.707106781186548,0.707106781186547,-8.65956056235494E-17));
#3987=DIRECTION('center_axis',(0.,-1.,0.));
#3988=DIRECTION('ref_axis',(0.,0.,-1.));
#3989=DIRECTION('center_axis',(0.,-1.,0.));
#3990=DIRECTION('ref_axis',(1.,0.,0.));
#3991=DIRECTION('',(0.,1.,0.));
#3992=DIRECTION('axis',(0.,0.,1.));
#3993=DIRECTION('refdir',(1.,0.,0.));
#3994=DIRECTION('center_axis',(0.,0.,1.));
#3995=DIRECTION('ref_axis',(1.,0.,0.));
#3996=DIRECTION('center_axis',(1.22464679914735E-16,-1.,0.));
#3997=DIRECTION('ref_axis',(-1.,-1.22464679914735E-16,0.));
#3998=DIRECTION('center_axis',(0.707106781186548,0.,0.707106781186548));
#3999=DIRECTION('ref_axis',(0.707106781186548,0.,-0.707106781186548));
#4000=DIRECTION('center_axis',(8.65956056235494E-17,-1.,-8.65956056235493E-17));
#4001=DIRECTION('ref_axis',(-0.707106781186547,-1.22464679914735E-16,0.707106781186547));
#4002=DIRECTION('center_axis',(1.,0.,0.));
#4003=DIRECTION('ref_axis',(6.12323399573676E-17,0.,-1.));
#4004=DIRECTION('center_axis',(7.49879891330929E-33,-1.,-1.22464679914735E-16));
#4005=DIRECTION('ref_axis',(-6.12323399573676E-17,-1.22464679914735E-16,
1.));
#4006=DIRECTION('center_axis',(0.707106781186548,0.,-0.707106781186548));
#4007=DIRECTION('ref_axis',(-0.707106781186548,0.,-0.707106781186548));
#4008=DIRECTION('center_axis',(-8.65956056235493E-17,-1.,-8.65956056235494E-17));
#4009=DIRECTION('ref_axis',(0.707106781186547,-1.22464679914735E-16,0.707106781186547));
#4010=DIRECTION('center_axis',(0.,0.,-1.));
#4011=DIRECTION('ref_axis',(-1.,0.,-1.22464679914735E-16));
#4012=DIRECTION('center_axis',(-1.22464679914735E-16,-1.,-1.49975978266186E-32));
#4013=DIRECTION('ref_axis',(1.,-1.22464679914735E-16,1.22464679914735E-16));
#4014=DIRECTION('center_axis',(-0.707106781186547,0.,-0.707106781186548));
#4015=DIRECTION('ref_axis',(-0.707106781186548,0.,0.707106781186547));
#4016=DIRECTION('center_axis',(-8.65956056235493E-17,-1.,8.65956056235493E-17));
#4017=DIRECTION('ref_axis',(0.707106781186548,-1.22464679914735E-16,-0.707106781186547));
#4018=DIRECTION('center_axis',(-1.,0.,0.));
#4019=DIRECTION('ref_axis',(-1.83697019872103E-16,0.,1.));
#4020=DIRECTION('center_axis',(-2.24963967399279E-32,-1.,1.22464679914735E-16));
#4021=DIRECTION('ref_axis',(1.83697019872103E-16,-1.22464679914735E-16,
-1.));
#4022=DIRECTION('center_axis',(-0.707106781186548,0.,0.707106781186548));
#4023=DIRECTION('ref_axis',(0.707106781186547,0.,0.707106781186548));
#4024=DIRECTION('center_axis',(8.65956056235493E-17,-1.,8.65956056235493E-17));
#4025=DIRECTION('ref_axis',(-0.707106781186547,-1.22464679914735E-16,-0.707106781186548));
#4026=DIRECTION('axis',(0.,0.,1.));
#4027=DIRECTION('refdir',(1.,0.,0.));
#4028=DIRECTION('center_axis',(0.,0.,1.));
#4029=DIRECTION('ref_axis',(1.,0.,0.));
#4030=DIRECTION('center_axis',(0.,-1.,0.));
#4031=DIRECTION('ref_axis',(0.,0.,-1.));
#4032=DIRECTION('center_axis',(0.,-1.,0.));
#4033=DIRECTION('ref_axis',(0.,0.,-1.));
#4034=DIRECTION('center_axis',(0.,1.,0.));
#4035=DIRECTION('ref_axis',(1.,0.,0.));
#4036=DIRECTION('center_axis',(0.,1.,0.));
#4037=DIRECTION('ref_axis',(1.,0.,0.));
#4038=DIRECTION('center_axis',(0.,1.,0.));
#4039=DIRECTION('ref_axis',(1.,0.,0.));
#4040=DIRECTION('center_axis',(0.,1.,0.));
#4041=DIRECTION('ref_axis',(1.,0.,0.));
#4042=DIRECTION('',(0.,-1.,0.));
#4043=DIRECTION('center_axis',(0.,-1.,0.));
#4044=DIRECTION('ref_axis',(1.,0.,0.));
#4045=DIRECTION('center_axis',(0.,1.,0.));
#4046=DIRECTION('ref_axis',(1.,0.,0.));
#4047=DIRECTION('center_axis',(0.,1.,0.));
#4048=DIRECTION('ref_axis',(1.,0.,0.));
#4049=DIRECTION('center_axis',(0.,1.,0.));
#4050=DIRECTION('ref_axis',(1.,0.,0.));
#4051=DIRECTION('center_axis',(0.,1.,0.));
#4052=DIRECTION('ref_axis',(1.,0.,0.));
#4053=DIRECTION('center_axis',(0.,1.,0.));
#4054=DIRECTION('ref_axis',(1.,0.,0.));
#4055=DIRECTION('center_axis',(0.,1.,0.));
#4056=DIRECTION('ref_axis',(1.,0.,0.));
#4057=DIRECTION('center_axis',(0.,-1.,0.));
#4058=DIRECTION('ref_axis',(1.,0.,0.));
#4059=DIRECTION('center_axis',(0.,-1.,0.));
#4060=DIRECTION('ref_axis',(0.,0.,-1.));
#4061=DIRECTION('center_axis',(6.12323399573677E-17,0.,1.));
#4062=DIRECTION('ref_axis',(1.,0.,0.));
#4063=DIRECTION('center_axis',(0.,-1.,0.));
#4064=DIRECTION('ref_axis',(0.,0.,-1.));
#4065=DIRECTION('center_axis',(0.,1.,0.));
#4066=DIRECTION('ref_axis',(1.,0.,0.));
#4067=DIRECTION('center_axis',(0.,-1.,0.));
#4068=DIRECTION('ref_axis',(1.,0.,0.));
#4069=DIRECTION('center_axis',(0.,-1.,0.));
#4070=DIRECTION('ref_axis',(0.,0.,-1.));
#4071=DIRECTION('center_axis',(0.,0.,1.));
#4072=DIRECTION('ref_axis',(1.,0.,0.));
#4073=DIRECTION('center_axis',(0.,-1.,0.));
#4074=DIRECTION('ref_axis',(0.,0.,-1.));
#4075=DIRECTION('center_axis',(0.,1.,0.));
#4076=DIRECTION('ref_axis',(1.,0.,0.));
#4077=DIRECTION('center_axis',(0.,-1.,0.));
#4078=DIRECTION('ref_axis',(1.,0.,0.));
#4079=DIRECTION('center_axis',(0.,-1.,0.));
#4080=DIRECTION('ref_axis',(0.,0.,-1.));
#4081=DIRECTION('center_axis',(0.,0.,1.));
#4082=DIRECTION('ref_axis',(1.,0.,0.));
#4083=DIRECTION('center_axis',(0.,-1.,0.));
#4084=DIRECTION('ref_axis',(0.,0.,-1.));
#4085=DIRECTION('center_axis',(0.,1.,0.));
#4086=DIRECTION('ref_axis',(1.,0.,0.));
#4087=DIRECTION('center_axis',(0.,-1.,0.));
#4088=DIRECTION('ref_axis',(1.,0.,0.));
#4089=DIRECTION('center_axis',(0.,-1.,0.));
#4090=DIRECTION('ref_axis',(0.,0.,-1.));
#4091=DIRECTION('center_axis',(0.,0.,1.));
#4092=DIRECTION('ref_axis',(1.,0.,0.));
#4093=DIRECTION('center_axis',(0.,-1.,0.));
#4094=DIRECTION('ref_axis',(0.,0.,-1.));
#4095=DIRECTION('center_axis',(0.,1.,0.));
#4096=DIRECTION('ref_axis',(1.,0.,0.));
#4097=DIRECTION('center_axis',(0.,-1.,0.));
#4098=DIRECTION('ref_axis',(1.,0.,0.));
#4099=DIRECTION('center_axis',(0.,-1.,0.));
#4100=DIRECTION('ref_axis',(0.,0.,-1.));
#4101=DIRECTION('center_axis',(6.12323399573676E-17,0.,1.));
#4102=DIRECTION('ref_axis',(1.,0.,0.));
#4103=DIRECTION('center_axis',(0.,-1.,0.));
#4104=DIRECTION('ref_axis',(0.,0.,-1.));
#4105=DIRECTION('center_axis',(0.,1.,0.));
#4106=DIRECTION('ref_axis',(1.,0.,0.));
#4107=DIRECTION('center_axis',(0.,-1.,0.));
#4108=DIRECTION('ref_axis',(1.,0.,0.));
#4109=DIRECTION('center_axis',(0.,-1.,0.));
#4110=DIRECTION('ref_axis',(0.,0.,-1.));
#4111=DIRECTION('center_axis',(0.,0.,1.));
#4112=DIRECTION('ref_axis',(1.,0.,0.));
#4113=DIRECTION('center_axis',(0.,-1.,0.));
#4114=DIRECTION('ref_axis',(0.,0.,-1.));
#4115=DIRECTION('center_axis',(0.,1.,0.));
#4116=DIRECTION('ref_axis',(1.,0.,0.));
#4117=DIRECTION('center_axis',(0.,1.,0.));
#4118=DIRECTION('ref_axis',(1.,0.,0.));
#4119=DIRECTION('',(0.,1.,0.));
#4120=DIRECTION('center_axis',(0.,-1.,0.));
#4121=DIRECTION('ref_axis',(1.,0.,0.));
#4122=DIRECTION('center_axis',(0.,-1.,0.));
#4123=DIRECTION('ref_axis',(1.,0.,0.));
#4124=DIRECTION('center_axis',(0.,1.,0.));
#4125=DIRECTION('ref_axis',(1.,0.,0.));
#4126=DIRECTION('center_axis',(0.,-1.,0.));
#4127=DIRECTION('ref_axis',(0.,0.,-1.));
#4128=DIRECTION('center_axis',(0.,0.,1.));
#4129=DIRECTION('ref_axis',(1.,0.,0.));
#4130=DIRECTION('center_axis',(0.,-1.,0.));
#4131=DIRECTION('ref_axis',(0.,0.,-1.));
#4132=DIRECTION('center_axis',(0.,-1.,0.));
#4133=DIRECTION('ref_axis',(-1.,0.,0.));
#4134=DIRECTION('center_axis',(0.,1.,0.));
#4135=DIRECTION('ref_axis',(1.,0.,0.));
#4136=DIRECTION('axis',(0.,0.,1.));
#4137=DIRECTION('refdir',(1.,0.,0.));
#4138=DIRECTION('center_axis',(0.,1.,0.));
#4139=DIRECTION('ref_axis',(0.,0.,1.));
#4140=DIRECTION('center_axis',(0.,-1.,0.));
#4141=DIRECTION('ref_axis',(1.,0.,0.));
#4142=DIRECTION('center_axis',(0.,-1.,0.));
#4143=DIRECTION('ref_axis',(1.,0.,0.));
#4144=DIRECTION('center_axis',(0.,-1.,0.));
#4145=DIRECTION('ref_axis',(1.,0.,0.));
#4146=DIRECTION('center_axis',(0.,-1.,0.));
#4147=DIRECTION('ref_axis',(1.,0.,0.));
#4148=DIRECTION('',(0.,1.,0.));
#4149=DIRECTION('center_axis',(0.,-1.,0.));
#4150=DIRECTION('ref_axis',(0.,0.,-1.));
#4151=DIRECTION('center_axis',(0.,-1.,0.));
#4152=DIRECTION('ref_axis',(1.,0.,0.));
#4153=DIRECTION('center_axis',(0.,-1.,0.));
#4154=DIRECTION('ref_axis',(1.,0.,0.));
#4155=DIRECTION('',(0.,1.,0.));
#4156=DIRECTION('center_axis',(0.,1.,0.));
#4157=DIRECTION('ref_axis',(0.,0.,1.));
#4158=DIRECTION('center_axis',(0.,-1.,0.));
#4159=DIRECTION('ref_axis',(1.,0.,0.));
#4160=DIRECTION('center_axis',(0.,-1.,0.));
#4161=DIRECTION('ref_axis',(1.,0.,0.));
#4162=DIRECTION('center_axis',(0.,-1.,0.));
#4163=DIRECTION('ref_axis',(1.,0.,0.));
#4164=DIRECTION('center_axis',(0.,-1.,0.));
#4165=DIRECTION('ref_axis',(1.,0.,0.));
#4166=DIRECTION('',(0.,1.,0.));
#4167=DIRECTION('center_axis',(0.,-1.,0.));
#4168=DIRECTION('ref_axis',(0.,0.,-1.));
#4169=DIRECTION('center_axis',(0.,-1.,0.));
#4170=DIRECTION('ref_axis',(1.,0.,0.));
#4171=DIRECTION('center_axis',(0.,-1.,0.));
#4172=DIRECTION('ref_axis',(1.,0.,0.));
#4173=DIRECTION('',(0.,1.,0.));
#4174=DIRECTION('',(0.,0.,1.));
#4175=DIRECTION('',(1.,0.,0.));
#4176=DIRECTION('',(0.,0.,1.));
#4177=DIRECTION('',(1.,0.,0.));
#4178=DIRECTION('',(0.,0.,1.));
#4179=DIRECTION('',(1.,0.,0.));
#4180=DIRECTION('',(0.,0.,1.));
#4181=DIRECTION('',(1.,0.,0.));
#4182=DIRECTION('',(0.,0.,1.));
#4183=DIRECTION('',(1.,0.,0.));
#4184=DIRECTION('',(0.,0.,1.));
#4185=DIRECTION('',(1.,0.,0.));
#4186=DIRECTION('',(0.,0.,1.));
#4187=DIRECTION('',(1.,0.,0.));
#4188=DIRECTION('',(0.,0.,1.));
#4189=DIRECTION('',(1.,0.,0.));
#4190=DIRECTION('',(0.,0.,1.));
#4191=DIRECTION('',(1.,0.,0.));
#4192=DIRECTION('',(0.,0.,1.));
#4193=DIRECTION('',(1.,0.,0.));
#4194=DIRECTION('',(0.,0.,1.));
#4195=DIRECTION('',(1.,0.,0.));
#4196=DIRECTION('',(0.,0.,1.));
#4197=DIRECTION('',(1.,0.,0.));
#4198=DIRECTION('',(0.,0.,1.));
#4199=DIRECTION('',(1.,0.,0.));
#4200=CARTESIAN_POINT('',(0.,0.,0.));
#4201=CARTESIAN_POINT('',(0.,0.,0.));
#4202=CARTESIAN_POINT('',(0.,0.,0.));
#4203=CARTESIAN_POINT('Origin',(-2.,0.,9.6));
#4204=CARTESIAN_POINT('',(-2.6,-7.34788079488412E-17,9.7));
#4205=CARTESIAN_POINT('Origin',(-2.,0.,9.7));
#4206=CARTESIAN_POINT('',(-2.6,7.34788079488412E-17,10.5));
#4207=CARTESIAN_POINT('',(-2.6,-7.34788079488412E-17,9.6));
#4208=CARTESIAN_POINT('Origin',(-2.,0.,10.5));
#4209=CARTESIAN_POINT('Origin',(1.,-2.5,9.6));
#4210=CARTESIAN_POINT('',(0.575,-2.5,9.7));
#4211=CARTESIAN_POINT('Origin',(1.,-2.5,9.7));
#4212=CARTESIAN_POINT('',(0.575,-2.5,10.5));
#4213=CARTESIAN_POINT('',(0.575,-2.5,9.6));
#4214=CARTESIAN_POINT('Origin',(1.,-2.5,10.5));
#4215=CARTESIAN_POINT('Origin',(-5.,2.5,9.6));
#4216=CARTESIAN_POINT('',(-5.425,2.5,9.7));
#4217=CARTESIAN_POINT('Origin',(-5.,2.5,9.7));
#4218=CARTESIAN_POINT('',(-5.425,2.5,10.5));
#4219=CARTESIAN_POINT('',(-5.425,2.5,9.6));
#4220=CARTESIAN_POINT('Origin',(-5.,2.5,10.5));
#4221=CARTESIAN_POINT('Origin',(-5.,-2.5,9.6));
#4222=CARTESIAN_POINT('',(-5.425,-2.5,9.7));
#4223=CARTESIAN_POINT('Origin',(-5.,-2.5,9.7));
#4224=CARTESIAN_POINT('',(-5.425,-2.5,10.5));
#4225=CARTESIAN_POINT('',(-5.425,-2.5,9.6));
#4226=CARTESIAN_POINT('Origin',(-5.,-2.5,10.5));
#4227=CARTESIAN_POINT('Origin',(1.,2.5,9.6));
#4228=CARTESIAN_POINT('',(0.575,2.5,9.7));
#4229=CARTESIAN_POINT('Origin',(1.,2.5,9.7));
#4230=CARTESIAN_POINT('',(0.575,2.5,10.5));
#4231=CARTESIAN_POINT('',(0.575,2.5,9.6));
#4232=CARTESIAN_POINT('Origin',(1.,2.5,10.5));
#4233=CARTESIAN_POINT('Origin',(2.,3.5,9.7));
#4234=CARTESIAN_POINT('',(2.,3.5,9.7));
#4235=CARTESIAN_POINT('',(-6.,3.5,9.7));
#4236=CARTESIAN_POINT('',(2.,3.5,9.7));
#4237=CARTESIAN_POINT('',(-6.,3.5,10.5));
#4238=CARTESIAN_POINT('',(-6.,3.5,9.7));
#4239=CARTESIAN_POINT('',(2.,3.5,10.5));
#4240=CARTESIAN_POINT('',(2.,3.5,10.5));
#4241=CARTESIAN_POINT('',(2.,3.5,9.7));
#4242=CARTESIAN_POINT('Origin',(2.,-3.5,9.7));
#4243=CARTESIAN_POINT('',(2.,-3.5,9.7));
#4244=CARTESIAN_POINT('',(2.,-3.5,9.7));
#4245=CARTESIAN_POINT('',(2.,-3.5,10.5));
#4246=CARTESIAN_POINT('',(2.,-3.5,10.5));
#4247=CARTESIAN_POINT('',(2.,-3.5,9.7));
#4248=CARTESIAN_POINT('Origin',(-6.,-3.5,9.7));
#4249=CARTESIAN_POINT('',(-6.,-3.5,9.7));
#4250=CARTESIAN_POINT('',(-6.,-3.5,9.7));
#4251=CARTESIAN_POINT('',(-6.,-3.5,10.5));
#4252=CARTESIAN_POINT('',(-6.,-3.5,10.5));
#4253=CARTESIAN_POINT('',(-6.,-3.5,9.7));
#4254=CARTESIAN_POINT('Origin',(-6.,3.5,9.7));
#4255=CARTESIAN_POINT('',(-6.,3.5,9.7));
#4256=CARTESIAN_POINT('',(-6.,3.5,10.5));
#4257=CARTESIAN_POINT('Origin',(-2.,0.,10.5));
#4258=CARTESIAN_POINT('Origin',(-2.,0.,9.7));
#4259=CARTESIAN_POINT('',(0.,0.,0.));
#4260=CARTESIAN_POINT('Origin',(-2.,0.,7.5));
#4261=CARTESIAN_POINT('',(-2.4,-4.89858719658941E-17,8.5));
#4262=CARTESIAN_POINT('Origin',(-2.,0.,8.5));
#4263=CARTESIAN_POINT('',(-2.4,-4.89858719658941E-17,7.5));
#4264=CARTESIAN_POINT('',(-2.4,-4.89858719658941E-17,7.5));
#4265=CARTESIAN_POINT('Origin',(-2.,0.,7.5));
#4266=CARTESIAN_POINT('Origin',(-2.,0.,7.5));
#4267=CARTESIAN_POINT('Origin',(-2.,0.,10.5));
#4268=CARTESIAN_POINT('',(-3.,-1.22464679914735E-16,10.5));
#4269=CARTESIAN_POINT('Origin',(-2.,0.,10.5));
#4270=CARTESIAN_POINT('',(-2.6,-7.34788079488412E-17,10.5));
#4271=CARTESIAN_POINT('Origin',(-2.,0.,10.5));
#4272=CARTESIAN_POINT('Origin',(-2.,0.,10.5));
#4273=CARTESIAN_POINT('',(-3.,-1.22464679914735E-16,10.9));
#4274=CARTESIAN_POINT('Origin',(-2.,0.,10.9));
#4275=CARTESIAN_POINT('',(-3.,-1.22464679914735E-16,10.5));
#4276=CARTESIAN_POINT('Origin',(-2.,0.,10.9));
#4277=CARTESIAN_POINT('Origin',(-2.,0.,8.5));
#4278=CARTESIAN_POINT('',(-2.6,-7.34788079488412E-17,8.5));
#4279=CARTESIAN_POINT('',(-2.6,-7.34788079488412E-17,8.5));
#4280=CARTESIAN_POINT('Origin',(-2.,0.,8.5));
#4281=CARTESIAN_POINT('Origin',(-2.,0.,8.5));
#4282=CARTESIAN_POINT('',(0.,0.,0.));
#4283=CARTESIAN_POINT('Origin',(-2.,0.,9.5));
#4284=CARTESIAN_POINT('',(-2.605,-7.40911313484149E-17,9.7));
#4285=CARTESIAN_POINT('Origin',(-2.,0.,9.7));
#4286=CARTESIAN_POINT('',(-2.605,-7.40911313484149E-17,9.5));
#4287=CARTESIAN_POINT('',(-2.605,-7.40911313484149E-17,9.5));
#4288=CARTESIAN_POINT('Origin',(-2.,0.,9.5));
#4289=CARTESIAN_POINT('Origin',(-2.,0.,9.5));
#4290=CARTESIAN_POINT('',(-4.,-2.44929359829471E-16,9.7));
#4291=CARTESIAN_POINT('Origin',(-2.,0.,9.7));
#4292=CARTESIAN_POINT('',(-4.,-2.44929359829471E-16,9.5));
#4293=CARTESIAN_POINT('',(-4.,-2.44929359829471E-16,9.5));
#4294=CARTESIAN_POINT('Origin',(-2.,0.,9.5));
#4295=CARTESIAN_POINT('Origin',(-2.,0.,9.7));
#4296=CARTESIAN_POINT('Origin',(-2.,0.,9.5));
#4297=CARTESIAN_POINT('',(0.,0.,0.));
#4298=CARTESIAN_POINT('Origin',(0.,0.,0.));
#4299=CARTESIAN_POINT('',(-0.42,0.16,5.14351655641888E-17));
#4300=CARTESIAN_POINT('Origin',(0.,0.16,0.));
#4301=CARTESIAN_POINT('',(-0.42,0.,5.14351655641888E-17));
#4302=CARTESIAN_POINT('',(-0.42,0.,5.14351655641888E-17));
#4303=CARTESIAN_POINT('Origin',(0.,0.,0.));
#4304=CARTESIAN_POINT('Origin',(0.,0.,0.));
#4305=CARTESIAN_POINT('',(-0.8,0.16,9.79717439317883E-17));
#4306=CARTESIAN_POINT('Origin',(0.,0.16,0.));
#4307=CARTESIAN_POINT('',(-0.8,0.,9.79717439317883E-17));
#4308=CARTESIAN_POINT('',(-0.8,0.,9.79717439317883E-17));
#4309=CARTESIAN_POINT('Origin',(0.,0.,0.));
#4310=CARTESIAN_POINT('Origin',(0.,0.16,0.));
#4311=CARTESIAN_POINT('Origin',(0.,0.,0.));
#4312=CARTESIAN_POINT('',(0.,0.,0.));
#4313=CARTESIAN_POINT('Origin',(0.,0.067277284513851,0.));
#4314=CARTESIAN_POINT('',(-0.375277674973257,0.0768195421087395,0.65));
#4315=CARTESIAN_POINT('',(0.375277674973257,0.0768195421087395,0.65));
#4316=CARTESIAN_POINT('Ctrl Pts',(-0.375277674973257,0.0768195421087395,
0.65));
#4317=CARTESIAN_POINT('Ctrl Pts',(1.66533453693773E-13,-0.0315137912242439,
0.65));
#4318=CARTESIAN_POINT('Ctrl Pts',(0.375277674973257,0.0768195421087394,
0.65));
#4319=CARTESIAN_POINT('',(-0.750555349946514,0.0768195421087394,-9.19165206894919E-17));
#4320=CARTESIAN_POINT('Ctrl Pts',(-0.750555349946514,0.0768195421087394,
-9.19165206894919E-17));
#4321=CARTESIAN_POINT('Ctrl Pts',(-0.562916512459802,-0.0315137912242434,
0.325000000000144));
#4322=CARTESIAN_POINT('Ctrl Pts',(-0.375277674973257,0.0768195421087395,
0.65));
#4323=CARTESIAN_POINT('',(-0.6175,-2.77555756156289E-17,-7.5621939847349E-17));
#4324=CARTESIAN_POINT('',(-0.734027674973257,0.067277284513851,-8.98924642641573E-17));
#4325=CARTESIAN_POINT('Origin',(0.,0.,0.));
#4326=CARTESIAN_POINT('',(-0.375277674973257,0.0768195421087395,-0.65));
#4327=CARTESIAN_POINT('Ctrl Pts',(-0.375277674973257,0.0768195421087395,
-0.65));
#4328=CARTESIAN_POINT('Ctrl Pts',(-0.562916512459968,-0.0315137912242437,
-0.324999999999856));
#4329=CARTESIAN_POINT('Ctrl Pts',(-0.750555349946514,0.0768195421087395,
-9.19165206894919E-17));
#4330=CARTESIAN_POINT('',(0.375277674973257,0.0768195421087395,-0.65));
#4331=CARTESIAN_POINT('Ctrl Pts',(0.375277674973257,0.0768195421087395,
-0.65));
#4332=CARTESIAN_POINT('Ctrl Pts',(-1.66144875635155E-13,-0.0315137912242437,
-0.65));
#4333=CARTESIAN_POINT('Ctrl Pts',(-0.375277674973257,0.0768195421087395,
-0.65));
#4334=CARTESIAN_POINT('',(0.750555349946514,0.0768195421087394,0.));
#4335=CARTESIAN_POINT('Ctrl Pts',(0.750555349946514,0.0768195421087394,
0.));
#4336=CARTESIAN_POINT('Ctrl Pts',(0.562916512459802,-0.0315137912242436,
-0.325000000000144));
#4337=CARTESIAN_POINT('Ctrl Pts',(0.375277674973257,0.0768195421087395,
-0.65));
#4338=CARTESIAN_POINT('Ctrl Pts',(0.375277674973257,0.0768195421087394,
0.65));
#4339=CARTESIAN_POINT('Ctrl Pts',(0.562916512459968,-0.0315137912242439,
0.324999999999856));
#4340=CARTESIAN_POINT('Ctrl Pts',(0.750555349946514,0.0768195421087394,
0.));
#4341=CARTESIAN_POINT('Origin',(0.,0.612722715486149,0.));
#4342=CARTESIAN_POINT('',(-0.6175,0.68,-7.5621939847349E-17));
#4343=CARTESIAN_POINT('Origin',(0.,0.68,0.));
#4344=CARTESIAN_POINT('',(-0.750555349946514,0.603180457891261,-9.19165206894919E-17));
#4345=CARTESIAN_POINT('',(-0.734027674973257,0.612722715486149,-8.98924642641573E-17));
#4346=CARTESIAN_POINT('',(-0.375277674973257,0.603180457891261,0.65));
#4347=CARTESIAN_POINT('Ctrl Pts',(-0.375277674973257,0.603180457891261,
0.65));
#4348=CARTESIAN_POINT('Ctrl Pts',(-0.562916512459968,0.711513791224243,
0.324999999999856));
#4349=CARTESIAN_POINT('Ctrl Pts',(-0.750555349946514,0.603180457891261,
-9.19165206894919E-17));
#4350=CARTESIAN_POINT('',(0.375277674973257,0.603180457891261,0.65));
#4351=CARTESIAN_POINT('Ctrl Pts',(0.375277674973257,0.603180457891261,0.65));
#4352=CARTESIAN_POINT('Ctrl Pts',(-1.66755498298699E-13,0.711513791224244,
0.65));
#4353=CARTESIAN_POINT('Ctrl Pts',(-0.375277674973257,0.603180457891261,
0.65));
#4354=CARTESIAN_POINT('',(0.750555349946514,0.603180457891261,0.));
#4355=CARTESIAN_POINT('Ctrl Pts',(0.750555349946514,0.603180457891261,0.));
#4356=CARTESIAN_POINT('Ctrl Pts',(0.562916512459802,0.711513791224244,0.325000000000144));
#4357=CARTESIAN_POINT('Ctrl Pts',(0.375277674973257,0.603180457891261,0.65));
#4358=CARTESIAN_POINT('',(0.375277674973257,0.603180457891261,-0.65));
#4359=CARTESIAN_POINT('Ctrl Pts',(0.375277674973257,0.603180457891261,-0.65));
#4360=CARTESIAN_POINT('Ctrl Pts',(0.562916512459969,0.711513791224244,-0.324999999999856));
#4361=CARTESIAN_POINT('Ctrl Pts',(0.750555349946514,0.603180457891261,0.));
#4362=CARTESIAN_POINT('',(-0.375277674973257,0.603180457891261,-0.65));
#4363=CARTESIAN_POINT('Ctrl Pts',(-0.375277674973257,0.603180457891261,
-0.65));
#4364=CARTESIAN_POINT('Ctrl Pts',(1.66422431391311E-13,0.711513791224244,
-0.65));
#4365=CARTESIAN_POINT('Ctrl Pts',(0.375277674973257,0.603180457891261,-0.65));
#4366=CARTESIAN_POINT('Ctrl Pts',(-0.750555349946514,0.603180457891261,
-9.19165206894919E-17));
#4367=CARTESIAN_POINT('Ctrl Pts',(-0.562916512459802,0.711513791224244,
-0.325000000000144));
#4368=CARTESIAN_POINT('Ctrl Pts',(-0.375277674973257,0.603180457891261,
-0.65));
#4369=CARTESIAN_POINT('Origin',(0.375277674973257,0.,-0.65));
#4370=CARTESIAN_POINT('',(-0.375277674973257,0.,-0.65));
#4371=CARTESIAN_POINT('',(0.375277674973257,0.,-0.65));
#4372=CARTESIAN_POINT('Origin',(-0.375277674973257,0.,-0.65));
#4373=CARTESIAN_POINT('',(-0.750555349946514,0.,-9.19165206894919E-17));
#4374=CARTESIAN_POINT('Origin',(-0.750555349946514,0.,-9.19165206894919E-17));
#4375=CARTESIAN_POINT('',(-0.375277674973257,0.,0.65));
#4376=CARTESIAN_POINT('Origin',(0.,0.,0.));
#4377=CARTESIAN_POINT('',(-0.338975,0.68,4.15124648740974E-17));
#4378=CARTESIAN_POINT('Origin',(0.,0.68,0.));
#4379=CARTESIAN_POINT('',(-0.338975,0.,4.15124648740974E-17));
#4380=CARTESIAN_POINT('',(-0.338975,0.,4.15124648740974E-17));
#4381=CARTESIAN_POINT('Origin',(0.,0.,0.));
#4382=CARTESIAN_POINT('Origin',(-0.375277674973257,0.,0.65));
#4383=CARTESIAN_POINT('',(0.375277674973257,0.,0.65));
#4384=CARTESIAN_POINT('Origin',(0.750555349946514,0.,0.));
#4385=CARTESIAN_POINT('',(0.750555349946514,0.,0.));
#4386=CARTESIAN_POINT('Origin',(0.375277674973257,0.,0.65));
#4387=CARTESIAN_POINT('Origin',(0.,0.68,-1.11022302462516E-16));
#4388=CARTESIAN_POINT('Origin',(0.,0.,-1.11022302462516E-16));
#4389=CARTESIAN_POINT('',(0.,0.,0.));
#4390=CARTESIAN_POINT('',(0.,0.,0.));
#4391=CARTESIAN_POINT('',(0.,0.,0.));
#4392=CARTESIAN_POINT('',(-2.,0.,8.5));
#4393=CARTESIAN_POINT('',(-2.,0.,8.34));
#4394=CARTESIAN_POINT('',(0.,0.,0.));
#4395=CARTESIAN_POINT('',(0.,0.,0.));
#4396=CARTESIAN_POINT('Origin',(-2.,0.,8.4));
#4397=CARTESIAN_POINT('',(-2.8,-9.79717439317883E-17,8.5));
#4398=CARTESIAN_POINT('Origin',(-2.,0.,8.5));
#4399=CARTESIAN_POINT('',(-2.8,9.79717439317883E-17,9.3));
#4400=CARTESIAN_POINT('',(-2.8,-9.79717439317883E-17,8.4));
#4401=CARTESIAN_POINT('Origin',(-2.,0.,9.3));
#4402=CARTESIAN_POINT('Origin',(0.,-2.3,4.));
#4403=CARTESIAN_POINT('',(0.5,-1.8,4.));
#4404=CARTESIAN_POINT('',(-0.5,-1.8,4.));
#4405=CARTESIAN_POINT('Origin',(0.,-1.8,4.));
#4406=CARTESIAN_POINT('',(0.5,-2.2,4.));
#4407=CARTESIAN_POINT('',(0.5,-2.3,4.));
#4408=CARTESIAN_POINT('',(-0.5,-2.2,4.));
#4409=CARTESIAN_POINT('Origin',(0.,-2.2,4.));
#4410=CARTESIAN_POINT('',(-0.5,-2.3,4.));
#4411=CARTESIAN_POINT('Origin',(0.,-2.3,4.));
#4412=CARTESIAN_POINT('',(-0.5,2.2,4.));
#4413=CARTESIAN_POINT('',(-0.5,1.8,4.));
#4414=CARTESIAN_POINT('',(-0.5,-2.3,4.));
#4415=CARTESIAN_POINT('',(0.5,2.2,4.));
#4416=CARTESIAN_POINT('Origin',(0.,2.2,4.));
#4417=CARTESIAN_POINT('',(0.5,1.8,4.));
#4418=CARTESIAN_POINT('',(0.5,-2.3,4.));
#4419=CARTESIAN_POINT('Origin',(0.,1.8,4.));
#4420=CARTESIAN_POINT('Origin',(2.,2.2,8.5));
#4421=CARTESIAN_POINT('',(-2.,2.2,4.));
#4422=CARTESIAN_POINT('',(-2.,2.2,4.));
#4423=CARTESIAN_POINT('',(-2.,2.2,8.5));
#4424=CARTESIAN_POINT('',(-2.,2.2,8.9));
#4425=CARTESIAN_POINT('',(-4.,2.2,8.5));
#4426=CARTESIAN_POINT('',(2.,2.2,8.5));
#4427=CARTESIAN_POINT('',(-4.,2.2,9.3));
#4428=CARTESIAN_POINT('',(-4.,2.2,8.5));
#4429=CARTESIAN_POINT('',(2.,2.2,9.3));
#4430=CARTESIAN_POINT('',(2.,2.2,9.3));
#4431=CARTESIAN_POINT('',(2.,2.2,4.));
#4432=CARTESIAN_POINT('',(2.,2.2,8.5));
#4433=CARTESIAN_POINT('',(-2.,2.2,4.));
#4434=CARTESIAN_POINT('Origin',(2.,1.8,4.));
#4435=CARTESIAN_POINT('',(-2.,1.8,4.));
#4436=CARTESIAN_POINT('',(-2.,1.8,4.));
#4437=CARTESIAN_POINT('',(-2.,1.8,4.));
#4438=CARTESIAN_POINT('Origin',(2.,1.8,4.));
#4439=CARTESIAN_POINT('',(2.,1.8,4.));
#4440=CARTESIAN_POINT('',(2.,1.8,4.));
#4441=CARTESIAN_POINT('',(-2.,1.8,4.));
#4442=CARTESIAN_POINT('Origin',(-4.,-2.2,8.5));
#4443=CARTESIAN_POINT('',(2.,-2.2,4.));
#4444=CARTESIAN_POINT('',(-2.,-2.2,4.));
#4445=CARTESIAN_POINT('',(2.,-2.2,9.3));
#4446=CARTESIAN_POINT('',(2.,-2.2,8.5));
#4447=CARTESIAN_POINT('',(-4.,-2.2,9.3));
#4448=CARTESIAN_POINT('',(-4.,-2.2,9.3));
#4449=CARTESIAN_POINT('',(-4.,-2.2,8.5));
#4450=CARTESIAN_POINT('',(-4.,-2.2,8.5));
#4451=CARTESIAN_POINT('',(-2.,-2.2,8.5));
#4452=CARTESIAN_POINT('',(-4.,-2.2,8.5));
#4453=CARTESIAN_POINT('',(-2.,-2.2,4.));
#4454=CARTESIAN_POINT('',(-2.,-2.2,8.9));
#4455=CARTESIAN_POINT('',(-2.,-2.2,4.));
#4456=CARTESIAN_POINT('Origin',(2.,-2.2,4.));
#4457=CARTESIAN_POINT('',(2.,-1.8,4.));
#4458=CARTESIAN_POINT('',(-2.,-1.8,4.));
#4459=CARTESIAN_POINT('',(2.,-2.2,4.));
#4460=CARTESIAN_POINT('Origin',(-2.,1.8,4.));
#4461=CARTESIAN_POINT('',(-2.,1.8,8.5));
#4462=CARTESIAN_POINT('',(-2.,0.9,8.5));
#4463=CARTESIAN_POINT('',(-2.,1.8,8.9));
#4464=CARTESIAN_POINT('Origin',(0.,1.8,6.45));
#4465=CARTESIAN_POINT('',(2.,1.8,8.5));
#4466=CARTESIAN_POINT('',(2.,1.8,4.));
#4467=CARTESIAN_POINT('',(-0.5,1.8,8.5));
#4468=CARTESIAN_POINT('Origin',(-1.,0.,8.5));
#4469=CARTESIAN_POINT('',(2.,-1.8,8.5));
#4470=CARTESIAN_POINT('',(2.,-2.2,8.5));
#4471=CARTESIAN_POINT('',(-2.,-1.8,8.5));
#4472=CARTESIAN_POINT('',(-0.5,-1.8,8.5));
#4473=CARTESIAN_POINT('',(-2.,-1.1,8.5));
#4474=CARTESIAN_POINT('',(-4.,2.2,8.5));
#4475=CARTESIAN_POINT('Origin',(2.,-2.2,8.5));
#4476=CARTESIAN_POINT('',(2.,-2.2,9.3));
#4477=CARTESIAN_POINT('',(2.,-1.8,4.));
#4478=CARTESIAN_POINT('Origin',(0.,-1.8,6.45));
#4479=CARTESIAN_POINT('',(-2.,-1.8,4.));
#4480=CARTESIAN_POINT('',(-2.,-1.8,4.));
#4481=CARTESIAN_POINT('',(-2.,-1.8,8.9));
#4482=CARTESIAN_POINT('Origin',(-2.,-2.2,4.));
#4483=CARTESIAN_POINT('',(-2.,-2.2,4.));
#4484=CARTESIAN_POINT('Origin',(2.,-2.2,4.));
#4485=CARTESIAN_POINT('Origin',(-4.,2.2,8.5));
#4486=CARTESIAN_POINT('',(-4.,2.2,9.3));
#4487=CARTESIAN_POINT('Origin',(-1.,0.,9.3));
#4488=CARTESIAN_POINT('',(0.,0.,0.));
#4489=CARTESIAN_POINT('Origin',(-2.,0.,8.5));
#4490=CARTESIAN_POINT('',(-2.605,-7.40911313484149E-17,9.3));
#4491=CARTESIAN_POINT('Origin',(-2.,0.,9.3));
#4492=CARTESIAN_POINT('',(-2.605,-7.40911313484149E-17,8.5));
#4493=CARTESIAN_POINT('',(-2.605,-7.40911313484149E-17,8.5));
#4494=CARTESIAN_POINT('Origin',(-2.,0.,8.5));
#4495=CARTESIAN_POINT('Origin',(-2.,0.,8.5));
#4496=CARTESIAN_POINT('',(-2.8,-9.79717439317883E-17,9.3));
#4497=CARTESIAN_POINT('Origin',(-2.,0.,9.3));
#4498=CARTESIAN_POINT('',(-2.8,-9.79717439317883E-17,8.5));
#4499=CARTESIAN_POINT('',(-2.8,-9.79717439317883E-17,8.5));
#4500=CARTESIAN_POINT('Origin',(-2.,0.,8.5));
#4501=CARTESIAN_POINT('Origin',(-2.,0.,9.3));
#4502=CARTESIAN_POINT('Origin',(-2.,0.,8.5));
#4503=CARTESIAN_POINT('',(0.,0.,0.));
#4504=CARTESIAN_POINT('Origin',(-2.,0.,9.3));
#4505=CARTESIAN_POINT('',(-2.8,-9.79717439317883E-17,9.5));
#4506=CARTESIAN_POINT('Origin',(-2.,0.,9.5));
#4507=CARTESIAN_POINT('',(-2.8,-9.79717439317883E-17,9.3));
#4508=CARTESIAN_POINT('',(-2.8,-9.79717439317883E-17,9.3));
#4509=CARTESIAN_POINT('Origin',(-2.,0.,9.3));
#4510=CARTESIAN_POINT('Origin',(-2.,0.,9.3));
#4511=CARTESIAN_POINT('',(-4.,-2.44929359829471E-16,9.5));
#4512=CARTESIAN_POINT('Origin',(-2.,0.,9.5));
#4513=CARTESIAN_POINT('',(-4.,-2.44929359829471E-16,9.3));
#4514=CARTESIAN_POINT('',(-4.,-2.44929359829471E-16,9.3));
#4515=CARTESIAN_POINT('Origin',(-2.,0.,9.3));
#4516=CARTESIAN_POINT('Origin',(-2.,0.,9.5));
#4517=CARTESIAN_POINT('Origin',(-2.,0.,9.3));
#4518=CARTESIAN_POINT('',(0.,0.,0.));
#4519=CARTESIAN_POINT('Origin',(-2.,0.,9.3));
#4520=CARTESIAN_POINT('',(-4.,-2.44929359829471E-16,9.7));
#4521=CARTESIAN_POINT('Origin',(-2.,0.,9.7));
#4522=CARTESIAN_POINT('',(-4.,-2.44929359829471E-16,9.3));
#4523=CARTESIAN_POINT('',(-4.,-2.44929359829471E-16,9.3));
#4524=CARTESIAN_POINT('Origin',(-2.,0.,9.3));
#4525=CARTESIAN_POINT('Origin',(-2.,0.,9.3));
#4526=CARTESIAN_POINT('',(-4.2,-2.69422295812418E-16,9.7));
#4527=CARTESIAN_POINT('Origin',(-2.,0.,9.7));
#4528=CARTESIAN_POINT('',(-4.2,-2.69422295812418E-16,9.3));
#4529=CARTESIAN_POINT('',(-4.2,-2.69422295812418E-16,9.3));
#4530=CARTESIAN_POINT('Origin',(-2.,0.,9.3));
#4531=CARTESIAN_POINT('Origin',(-2.,0.,9.7));
#4532=CARTESIAN_POINT('Origin',(-2.,0.,9.3));
#4533=CARTESIAN_POINT('',(0.,0.,0.));
#4534=CARTESIAN_POINT('Origin',(0.,1.1,4.));
#4535=CARTESIAN_POINT('',(-0.165,1.1,4.));
#4536=CARTESIAN_POINT('Origin',(0.,1.1,4.));
#4537=CARTESIAN_POINT('',(-0.165,2.2,4.));
#4538=CARTESIAN_POINT('',(-0.165,1.1,4.));
#4539=CARTESIAN_POINT('Origin',(0.,2.2,4.));
#4540=CARTESIAN_POINT('Origin',(0.,1.1,4.));
#4541=CARTESIAN_POINT('Origin',(0.,-2.2,4.));
#4542=CARTESIAN_POINT('',(-0.8,-2.2,4.));
#4543=CARTESIAN_POINT('Origin',(0.,-2.2,4.));
#4544=CARTESIAN_POINT('',(-0.5,-2.2,4.));
#4545=CARTESIAN_POINT('Origin',(0.,-2.2,4.));
#4546=CARTESIAN_POINT('Origin',(0.,-2.6,4.));
#4547=CARTESIAN_POINT('',(-0.8,-2.6,4.));
#4548=CARTESIAN_POINT('',(-0.8,-2.6,4.));
#4549=CARTESIAN_POINT('Origin',(0.,-2.6,4.));
#4550=CARTESIAN_POINT('Origin',(0.,-2.6,4.));
#4551=CARTESIAN_POINT('Origin',(0.,-2.2,4.));
#4552=CARTESIAN_POINT('',(-0.5,2.2,4.));
#4553=CARTESIAN_POINT('Origin',(0.,2.2,4.));
#4554=CARTESIAN_POINT('',(-0.5,-2.2,4.));
#4555=CARTESIAN_POINT('Origin',(0.,2.2,4.));
#4556=CARTESIAN_POINT('',(0.,0.,0.));
#4557=CARTESIAN_POINT('Origin',(0.,-1.8,4.));
#4558=CARTESIAN_POINT('',(-0.505,-1.05,4.));
#4559=CARTESIAN_POINT('Origin',(0.,-1.05,4.));
#4560=CARTESIAN_POINT('',(-0.505,-1.8,4.));
#4561=CARTESIAN_POINT('',(-0.505,-1.8,4.));
#4562=CARTESIAN_POINT('Origin',(0.,-1.8,4.));
#4563=CARTESIAN_POINT('Origin',(0.,-1.8,4.));
#4564=CARTESIAN_POINT('',(-0.7,-1.05,4.));
#4565=CARTESIAN_POINT('Origin',(0.,-1.05,4.));
#4566=CARTESIAN_POINT('',(-0.7,-1.8,4.));
#4567=CARTESIAN_POINT('',(-0.7,-1.8,4.));
#4568=CARTESIAN_POINT('Origin',(0.,-1.8,4.));
#4569=CARTESIAN_POINT('Origin',(0.,-1.05,4.));
#4570=CARTESIAN_POINT('Origin',(0.,-1.8,4.));
#4571=CARTESIAN_POINT('',(0.,0.,0.));
#4572=CARTESIAN_POINT('Origin',(0.,1.05,4.));
#4573=CARTESIAN_POINT('',(-0.505,1.8,4.));
#4574=CARTESIAN_POINT('Origin',(0.,1.8,4.));
#4575=CARTESIAN_POINT('',(-0.505,1.05,4.));
#4576=CARTESIAN_POINT('',(-0.505,1.05,4.));
#4577=CARTESIAN_POINT('Origin',(0.,1.05,4.));
#4578=CARTESIAN_POINT('Origin',(0.,1.05,4.));
#4579=CARTESIAN_POINT('',(-0.7,1.8,4.));
#4580=CARTESIAN_POINT('Origin',(0.,1.8,4.));
#4581=CARTESIAN_POINT('',(-0.7,1.05,4.));
#4582=CARTESIAN_POINT('',(-0.7,1.05,4.));
#4583=CARTESIAN_POINT('Origin',(0.,1.05,4.));
#4584=CARTESIAN_POINT('Origin',(0.,1.8,4.));
#4585=CARTESIAN_POINT('Origin',(0.,1.05,4.));
#4586=CARTESIAN_POINT('',(0.,0.,0.));
#4587=CARTESIAN_POINT('Origin',(0.,2.2,4.));
#4588=CARTESIAN_POINT('',(-0.225,2.4,4.));
#4589=CARTESIAN_POINT('Origin',(0.,2.4,4.));
#4590=CARTESIAN_POINT('',(-0.225,2.2,4.));
#4591=CARTESIAN_POINT('',(-0.225,2.2,4.));
#4592=CARTESIAN_POINT('Origin',(0.,2.2,4.));
#4593=CARTESIAN_POINT('Origin',(0.,2.2,4.));
#4594=CARTESIAN_POINT('',(-0.8,2.4,4.));
#4595=CARTESIAN_POINT('Origin',(0.,2.4,4.));
#4596=CARTESIAN_POINT('',(-0.8,2.2,4.));
#4597=CARTESIAN_POINT('',(-0.8,2.2,4.));
#4598=CARTESIAN_POINT('Origin',(0.,2.2,4.));
#4599=CARTESIAN_POINT('Origin',(0.,2.4,4.));
#4600=CARTESIAN_POINT('Origin',(0.,2.2,4.));
#4601=CARTESIAN_POINT('',(0.,0.,0.));
#4602=CARTESIAN_POINT('Origin',(0.0866025403784439,-0.4,-0.15));
#4603=CARTESIAN_POINT('',(0.173205080756888,-0.4,0.));
#4604=CARTESIAN_POINT('',(0.0866025403784439,-0.4,-0.15));
#4605=CARTESIAN_POINT('',(0.173205080756888,-0.4,0.));
#4606=CARTESIAN_POINT('',(0.0866025403784439,-0.64,-0.15));
#4607=CARTESIAN_POINT('',(0.0866025403784439,-0.4,-0.15));
#4608=CARTESIAN_POINT('',(0.173205080756888,-0.64,0.));
#4609=CARTESIAN_POINT('',(0.173205080756888,-0.64,0.));
#4610=CARTESIAN_POINT('',(0.173205080756888,-0.4,0.));
#4611=CARTESIAN_POINT('Origin',(-0.0866025403784438,-0.4,-0.15));
#4612=CARTESIAN_POINT('',(-0.0866025403784438,-0.4,-0.15));
#4613=CARTESIAN_POINT('',(0.0866025403784439,-0.4,-0.15));
#4614=CARTESIAN_POINT('',(-0.0866025403784438,-0.64,-0.15));
#4615=CARTESIAN_POINT('',(-0.0866025403784438,-0.4,-0.15));
#4616=CARTESIAN_POINT('',(0.0866025403784439,-0.64,-0.15));
#4617=CARTESIAN_POINT('Origin',(-0.173205080756888,-0.4,-2.77555756156289E-17));
#4618=CARTESIAN_POINT('',(-0.173205080756888,-0.4,-2.12115047744981E-17));
#4619=CARTESIAN_POINT('',(-0.0866025403784438,-0.4,-0.15));
#4620=CARTESIAN_POINT('',(-0.173205080756888,-0.64,-2.77555756156289E-17));
#4621=CARTESIAN_POINT('',(-0.173205080756888,-0.4,-2.12115047744981E-17));
#4622=CARTESIAN_POINT('',(-0.0866025403784438,-0.64,-0.15));
#4623=CARTESIAN_POINT('Origin',(-0.0866025403784439,-0.4,0.15));
#4624=CARTESIAN_POINT('',(-0.0866025403784439,-0.4,0.15));
#4625=CARTESIAN_POINT('',(-0.173205080756888,-0.4,-2.12115047744981E-17));
#4626=CARTESIAN_POINT('',(-0.0866025403784439,-0.64,0.15));
#4627=CARTESIAN_POINT('',(-0.0866025403784439,-0.4,0.15));
#4628=CARTESIAN_POINT('',(-0.173205080756888,-0.64,-2.12115047744981E-17));
#4629=CARTESIAN_POINT('Origin',(0.0866025403784439,-0.4,0.15));
#4630=CARTESIAN_POINT('',(0.0866025403784439,-0.4,0.15));
#4631=CARTESIAN_POINT('',(-0.0866025403784439,-0.4,0.15));
#4632=CARTESIAN_POINT('',(0.0866025403784439,-0.64,0.15));
#4633=CARTESIAN_POINT('',(0.0866025403784439,-0.4,0.15));
#4634=CARTESIAN_POINT('',(-0.0866025403784439,-0.64,0.15));
#4635=CARTESIAN_POINT('Origin',(0.173205080756888,-0.4,0.));
#4636=CARTESIAN_POINT('',(0.0866025403784439,-0.4,0.15));
#4637=CARTESIAN_POINT('',(0.0866025403784439,-0.64,0.15));
#4638=CARTESIAN_POINT('Origin',(0.,-0.4,-2.77555756156289E-17));
#4639=CARTESIAN_POINT('Origin',(0.,-0.64,-2.77555756156289E-17));
#4640=CARTESIAN_POINT('Origin',(0.,-1.,0.));
#4641=CARTESIAN_POINT('',(-0.1954,-1.,2.39295984553393E-17));
#4642=CARTESIAN_POINT('Origin',(0.,-1.,0.));
#4643=CARTESIAN_POINT('Origin',(0.3,0.4,0.));
#4644=CARTESIAN_POINT('',(-0.3,0.4,-3.67394039744206E-17));
#4645=CARTESIAN_POINT('Origin',(0.,0.4,0.));
#4646=CARTESIAN_POINT('Origin',(0.,0.375,0.));
#4647=CARTESIAN_POINT('',(-0.35,0.35,-4.28626379701573E-17));
#4648=CARTESIAN_POINT('Origin',(0.,0.35,0.));
#4649=CARTESIAN_POINT('',(-0.325,0.375,-3.9801020972289E-17));
#4650=CARTESIAN_POINT('Origin',(0.,0.19,0.));
#4651=CARTESIAN_POINT('',(-0.35,0.03,-4.28626379701574E-17));
#4652=CARTESIAN_POINT('Origin',(0.,0.03,0.));
#4653=CARTESIAN_POINT('',(-0.35,0.19,-4.28626379701574E-17));
#4654=CARTESIAN_POINT('Origin',(0.,0.0149999999999999,0.));
#4655=CARTESIAN_POINT('',(-0.32,-3.29597460435593E-17,-3.91886975727153E-17));
#4656=CARTESIAN_POINT('Origin',(0.,0.,0.));
#4657=CARTESIAN_POINT('',(-0.335,0.0149999999999999,-4.10256677714363E-17));
#4658=CARTESIAN_POINT('Origin',(0.22,0.,0.));
#4659=CARTESIAN_POINT('',(-0.22,-6.93889390390723E-18,-2.69422295812418E-17));
#4660=CARTESIAN_POINT('Origin',(0.,0.,0.));
#4661=CARTESIAN_POINT('Origin',(0.,-0.02,0.));
#4662=CARTESIAN_POINT('',(-0.1954,-0.0492,2.39295984553393E-17));
#4663=CARTESIAN_POINT('Origin',(0.,-0.0492,0.));
#4664=CARTESIAN_POINT('',(-0.21,-0.02,-2.57175827820944E-17));
#4665=CARTESIAN_POINT('Origin',(0.,-0.8,0.));
#4666=CARTESIAN_POINT('',(-0.1954,-0.8,-2.39295984553393E-17));
#4667=CARTESIAN_POINT('',(0.,0.,0.));
#4668=CARTESIAN_POINT('',(0.,0.,0.));
#4669=CARTESIAN_POINT('',(0.,0.,0.));
#4670=CARTESIAN_POINT('',(0.,0.,0.));
#4671=CARTESIAN_POINT('',(0.,0.,0.));
#4672=CARTESIAN_POINT('',(0.,0.,0.));
#4673=CARTESIAN_POINT('',(0.,0.,0.));
#4674=CARTESIAN_POINT('',(0.,0.,0.));
#4675=CARTESIAN_POINT('',(0.,2.4,4.));
#4676=CARTESIAN_POINT('',(0.,0.,0.));
#4677=CARTESIAN_POINT('',(0.,0.,0.));
#4678=CARTESIAN_POINT('Origin',(0.,0.15,4.));
#4679=CARTESIAN_POINT('',(-1.5,0.15,4.));
#4680=CARTESIAN_POINT('Origin',(0.,0.15,4.));
#4681=CARTESIAN_POINT('',(-1.5,1.2,4.));
#4682=CARTESIAN_POINT('',(-1.5,0.15,4.));
#4683=CARTESIAN_POINT('Origin',(0.,1.2,4.));
#4684=CARTESIAN_POINT('Origin',(0.,0.15,4.));
#4685=CARTESIAN_POINT('',(-0.52,0.15,4.));
#4686=CARTESIAN_POINT('Origin',(0.,0.15,4.));
#4687=CARTESIAN_POINT('Origin',(0.,-1.3,4.));
#4688=CARTESIAN_POINT('',(-1.5,-1.2,4.));
#4689=CARTESIAN_POINT('Origin',(0.,-1.2,4.));
#4690=CARTESIAN_POINT('',(-1.5,-0.15,4.));
#4691=CARTESIAN_POINT('',(-1.5,-1.3,4.));
#4692=CARTESIAN_POINT('Origin',(0.,-0.15,4.));
#4693=CARTESIAN_POINT('Origin',(0.,-0.15,4.));
#4694=CARTESIAN_POINT('',(-0.52,-0.15,4.));
#4695=CARTESIAN_POINT('Origin',(0.,-0.15,4.));
#4696=CARTESIAN_POINT('Origin',(0.,-1.2,4.));
#4697=CARTESIAN_POINT('',(-0.52,-1.2,4.));
#4698=CARTESIAN_POINT('Origin',(0.,-1.2,4.));
#4699=CARTESIAN_POINT('',(-3.75,1.2,4.));
#4700=CARTESIAN_POINT('Origin',(0.,1.2,4.));
#4701=CARTESIAN_POINT('',(-3.75,-1.2,4.));
#4702=CARTESIAN_POINT('',(-3.75,-1.2,4.));
#4703=CARTESIAN_POINT('Origin',(0.,-1.2,4.));
#4704=CARTESIAN_POINT('Origin',(0.,1.2,4.));
#4705=CARTESIAN_POINT('Origin',(0.,-1.2,4.));
#4706=CARTESIAN_POINT('',(0.,0.,0.));
#4707=CARTESIAN_POINT('Origin',(0.,-1.2,4.));
#4708=CARTESIAN_POINT('',(-1.1,-1.05,4.));
#4709=CARTESIAN_POINT('Origin',(0.,-1.05,4.));
#4710=CARTESIAN_POINT('',(-1.1,-1.2,4.));
#4711=CARTESIAN_POINT('',(-1.1,-1.2,4.));
#4712=CARTESIAN_POINT('Origin',(0.,-1.2,4.));
#4713=CARTESIAN_POINT('Origin',(0.,-1.2,4.));
#4714=CARTESIAN_POINT('',(-1.5,-1.05,4.));
#4715=CARTESIAN_POINT('Origin',(0.,-1.05,4.));
#4716=CARTESIAN_POINT('',(-1.5,-1.2,4.));
#4717=CARTESIAN_POINT('',(-1.5,-1.2,4.));
#4718=CARTESIAN_POINT('Origin',(0.,-1.2,4.));
#4719=CARTESIAN_POINT('Origin',(0.,-1.05,4.));
#4720=CARTESIAN_POINT('Origin',(0.,-1.2,4.));
#4721=CARTESIAN_POINT('',(0.,0.,0.));
#4722=CARTESIAN_POINT('Origin',(0.,1.05,4.));
#4723=CARTESIAN_POINT('',(-1.1,1.2,4.));
#4724=CARTESIAN_POINT('Origin',(0.,1.2,4.));
#4725=CARTESIAN_POINT('',(-1.1,1.05,4.));
#4726=CARTESIAN_POINT('',(-1.1,1.05,4.));
#4727=CARTESIAN_POINT('Origin',(0.,1.05,4.));
#4728=CARTESIAN_POINT('Origin',(0.,1.05,4.));
#4729=CARTESIAN_POINT('',(-1.5,1.2,4.));
#4730=CARTESIAN_POINT('Origin',(0.,1.2,4.));
#4731=CARTESIAN_POINT('',(-1.5,1.05,4.));
#4732=CARTESIAN_POINT('',(-1.5,1.05,4.));
#4733=CARTESIAN_POINT('Origin',(0.,1.05,4.));
#4734=CARTESIAN_POINT('Origin',(0.,1.2,4.));
#4735=CARTESIAN_POINT('Origin',(0.,1.05,4.));
#4736=CARTESIAN_POINT('',(0.,0.,0.));
#4737=CARTESIAN_POINT('',(0.,0.,0.));
#4738=CARTESIAN_POINT('Origin',(0.,0.,0.));
#4739=CARTESIAN_POINT('',(-0.976185,-0.246528389340863,-1.19548183562566E-16));
#4740=CARTESIAN_POINT('',(-1.19548183562566E-16,-0.246528389340863,0.976185));
#4741=CARTESIAN_POINT('Origin',(0.,-0.246528389340863,0.));
#4742=CARTESIAN_POINT('Origin',(0.,-0.246528389340863,0.));
#4743=CARTESIAN_POINT('',(-1.19548183562566E-16,0.246528389340863,0.976185));
#4744=CARTESIAN_POINT('Origin',(-1.22464679914735E-16,0.,1.));
#4745=CARTESIAN_POINT('',(-0.976185,0.246528389340863,1.19548183562566E-16));
#4746=CARTESIAN_POINT('Origin',(0.,0.246528389340863,0.));
#4747=CARTESIAN_POINT('Origin',(0.,0.246528389340863,0.));
#4748=CARTESIAN_POINT('Origin',(0.,0.,0.));
#4749=CARTESIAN_POINT('',(-0.976185,0.45,-1.19548183562566E-16));
#4750=CARTESIAN_POINT('',(-0.976185,0.,-1.19548183562566E-16));
#4751=CARTESIAN_POINT('Origin',(0.,0.45,0.));
#4752=CARTESIAN_POINT('Origin',(0.,0.,0.));
#4753=CARTESIAN_POINT('',(-0.5,-0.39,-6.12323399573677E-17));
#4754=CARTESIAN_POINT('Origin',(0.,-0.39,0.));
#4755=CARTESIAN_POINT('',(-0.5,0.39,-6.12323399573677E-17));
#4756=CARTESIAN_POINT('',(-0.5,0.,-6.12323399573677E-17));
#4757=CARTESIAN_POINT('Origin',(0.,0.39,0.));
#4758=CARTESIAN_POINT('Origin',(0.,0.42,0.));
#4759=CARTESIAN_POINT('',(-0.56,0.45,-6.85802207522518E-17));
#4760=CARTESIAN_POINT('',(-0.53,0.42,-6.49062803548097E-17));
#4761=CARTESIAN_POINT('Origin',(0.,0.45,0.));
#4762=CARTESIAN_POINT('Origin',(0.976185,0.45,0.));
#4763=CARTESIAN_POINT('Origin',(0.,0.,0.));
#4764=CARTESIAN_POINT('',(-0.976185,-0.45,-1.19548183562566E-16));
#4765=CARTESIAN_POINT('Origin',(0.,-0.45,0.));
#4766=CARTESIAN_POINT('',(-0.976185,0.,-1.19548183562566E-16));
#4767=CARTESIAN_POINT('Origin',(0.56,-0.45,0.));
#4768=CARTESIAN_POINT('',(-0.56,-0.45,-6.85802207522518E-17));
#4769=CARTESIAN_POINT('Origin',(0.,-0.45,0.));
#4770=CARTESIAN_POINT('Origin',(0.,-0.42,0.));
#4771=CARTESIAN_POINT('',(-0.53,-0.42,-6.49062803548097E-17));
#4772=CARTESIAN_POINT('',(0.,0.,0.));
#4773=CARTESIAN_POINT('Origin',(0.,0.,0.));
#4774=CARTESIAN_POINT('',(-1.023815,0.246528389340863,-1.25381176266905E-16));
#4775=CARTESIAN_POINT('',(-1.25381176266905E-16,0.246528389340863,1.023815));
#4776=CARTESIAN_POINT('Origin',(0.,0.246528389340863,0.));
#4777=CARTESIAN_POINT('Origin',(0.,0.246528389340863,0.));
#4778=CARTESIAN_POINT('',(-1.25381176266905E-16,-0.246528389340863,1.023815));
#4779=CARTESIAN_POINT('Origin',(-1.22464679914735E-16,0.,1.));
#4780=CARTESIAN_POINT('',(-1.023815,-0.246528389340863,1.25381176266905E-16));
#4781=CARTESIAN_POINT('Origin',(0.,-0.246528389340863,0.));
#4782=CARTESIAN_POINT('Origin',(0.,-0.246528389340863,0.));
#4783=CARTESIAN_POINT('Origin',(0.,0.,0.));
#4784=CARTESIAN_POINT('',(-1.023815,-0.45,-1.25381176266905E-16));
#4785=CARTESIAN_POINT('Origin',(0.,-0.45,0.));
#4786=CARTESIAN_POINT('',(-1.023815,0.,-1.25381176266905E-16));
#4787=CARTESIAN_POINT('Origin',(1.44,0.45,0.));
#4788=CARTESIAN_POINT('',(-1.44,0.45,-1.76349139077219E-16));
#4789=CARTESIAN_POINT('Origin',(0.,0.45,0.));
#4790=CARTESIAN_POINT('',(-1.023815,0.45,-1.25381176266905E-16));
#4791=CARTESIAN_POINT('Origin',(0.,0.45,0.));
#4792=CARTESIAN_POINT('Origin',(0.,0.42,0.));
#4793=CARTESIAN_POINT('',(-1.5,0.39,-1.83697019872103E-16));
#4794=CARTESIAN_POINT('Origin',(0.,0.39,0.));
#4795=CARTESIAN_POINT('',(-1.47,0.42,-1.80023079474661E-16));
#4796=CARTESIAN_POINT('Origin',(0.,0.,0.));
#4797=CARTESIAN_POINT('',(-1.5,-0.39,-1.83697019872103E-16));
#4798=CARTESIAN_POINT('Origin',(0.,-0.39,0.));
#4799=CARTESIAN_POINT('',(-1.5,0.,-1.83697019872103E-16));
#4800=CARTESIAN_POINT('Origin',(0.,-0.42,0.));
#4801=CARTESIAN_POINT('',(-1.44,-0.45,-1.76349139077219E-16));
#4802=CARTESIAN_POINT('Origin',(0.,-0.45,0.));
#4803=CARTESIAN_POINT('',(-1.47,-0.42,-1.80023079474661E-16));
#4804=CARTESIAN_POINT('Origin',(1.023815,-0.45,0.));
#4805=CARTESIAN_POINT('Origin',(0.,0.,0.));
#4806=CARTESIAN_POINT('',(-1.023815,0.,-1.25381176266905E-16));
#4807=CARTESIAN_POINT('',(0.,0.,0.));
#4808=CARTESIAN_POINT('Origin',(1.,0.,0.));
#4809=CARTESIAN_POINT('',(1.,-1.78583896120461E-33,0.23815));
#4810=CARTESIAN_POINT('',(1.,-1.78583896120461E-33,-0.23815));
#4811=CARTESIAN_POINT('Origin',(1.,0.,0.));
#4812=CARTESIAN_POINT('Origin',(0.707106781186548,0.,-0.707106781186547));
#4813=CARTESIAN_POINT('',(0.875504261126124,-1.78583896120461E-33,-0.538709301246971));
#4814=CARTESIAN_POINT('',(0.538709301246971,-1.78583896120461E-33,-0.875504261126124));
#4815=CARTESIAN_POINT('Origin',(0.707106781186548,0.,-0.707106781186547));
#4816=CARTESIAN_POINT('Origin',(6.12323399573677E-17,0.,-1.));
#4817=CARTESIAN_POINT('',(0.23815,-1.78583896120461E-33,-1.));
#4818=CARTESIAN_POINT('',(-0.23815,-1.78583896120461E-33,-1.));
#4819=CARTESIAN_POINT('Origin',(6.12323399573677E-17,0.,-1.));
#4820=CARTESIAN_POINT('Origin',(-0.707106781186547,0.,-0.707106781186548));
#4821=CARTESIAN_POINT('',(-0.538709301246971,-1.78583896120461E-33,-0.875504261126124));
#4822=CARTESIAN_POINT('',(-0.875504261126124,-1.78583896120461E-33,-0.538709301246971));
#4823=CARTESIAN_POINT('Origin',(-0.707106781186547,0.,-0.707106781186548));
#4824=CARTESIAN_POINT('Origin',(-1.,0.,-1.22464679914735E-16));
#4825=CARTESIAN_POINT('',(-1.,-1.78583896120461E-33,-0.23815));
#4826=CARTESIAN_POINT('',(-1.,-1.78583896120461E-33,0.23815));
#4827=CARTESIAN_POINT('Origin',(-1.,0.,-1.22464679914735E-16));
#4828=CARTESIAN_POINT('Origin',(-0.707106781186548,0.,0.707106781186547));
#4829=CARTESIAN_POINT('',(-0.875504261126124,-7.94881478324376E-33,0.538709301246971));
#4830=CARTESIAN_POINT('',(-0.538709301246971,4.37713686083455E-33,0.875504261126124));
#4831=CARTESIAN_POINT('Origin',(-0.707106781186548,0.,0.707106781186547));
#4832=CARTESIAN_POINT('Origin',(-1.83697019872103E-16,0.,1.));
#4833=CARTESIAN_POINT('',(-0.23815,-1.78583896120461E-33,1.));
#4834=CARTESIAN_POINT('',(0.23815,-1.78583896120461E-33,1.));
#4835=CARTESIAN_POINT('Origin',(-1.83697019872103E-16,0.,1.));
#4836=CARTESIAN_POINT('Origin',(0.707106781186547,0.,0.707106781186548));
#4837=CARTESIAN_POINT('',(0.538709301246971,-4.86732687222419E-33,0.875504261126124));
#4838=CARTESIAN_POINT('',(0.875504261126124,1.29564894981497E-33,0.538709301246971));
#4839=CARTESIAN_POINT('Origin',(0.707106781186547,0.,0.707106781186548));
#4840=CARTESIAN_POINT('',(0.,0.,0.));
#4841=CARTESIAN_POINT('Origin',(0.707106781186547,0.,0.707106781186548));
#4842=CARTESIAN_POINT('',(0.504455939115715,-0.04763,0.841298510752802));
#4843=CARTESIAN_POINT('',(0.841298510752802,-0.04763,0.504455939115715));
#4844=CARTESIAN_POINT('Ctrl Pts',(0.504455939115715,-0.04763,0.841298510752802));
#4845=CARTESIAN_POINT('Ctrl Pts',(0.508899795931835,-0.0740444353928835,
0.838633903678357));
#4846=CARTESIAN_POINT('Ctrl Pts',(0.517157748491652,-0.0999305678883309,
0.833661031856294));
#4847=CARTESIAN_POINT('Ctrl Pts',(0.537715343527944,-0.142345102874864,
0.820511285096538));
#4848=CARTESIAN_POINT('Ctrl Pts',(0.548874290046456,-0.159766064500479,
0.813159949759));
#4849=CARTESIAN_POINT('Ctrl Pts',(0.573915184558107,-0.190326085855194,
0.795684265985089));
#4850=CARTESIAN_POINT('Ctrl Pts',(0.587792702767295,-0.203463743702801,
0.78555112003688));
#4851=CARTESIAN_POINT('Ctrl Pts',(0.615966552324775,-0.224161999508995,
0.763642258217233));
#4852=CARTESIAN_POINT('Ctrl Pts',(0.631684198665438,-0.232861760990032,
0.750785745543687));
#4853=CARTESIAN_POINT('Ctrl Pts',(0.663382628119203,-0.244251601209411,
0.722929908501543));
#4854=CARTESIAN_POINT('Ctrl Pts',(0.679352081686668,-0.246942143572133,
0.707917883896095));
#4855=CARTESIAN_POINT('Ctrl Pts',(0.707917883896095,-0.246942143572133,
0.679352081686668));
#4856=CARTESIAN_POINT('Ctrl Pts',(0.722929908501543,-0.244251601209411,
0.663382628119203));
#4857=CARTESIAN_POINT('Ctrl Pts',(0.750785745543687,-0.232861760990032,
0.631684198665439));
#4858=CARTESIAN_POINT('Ctrl Pts',(0.763642258217232,-0.224161999508995,
0.615966552324775));
#4859=CARTESIAN_POINT('Ctrl Pts',(0.78555112003688,-0.203463743702801,0.587792702767295));
#4860=CARTESIAN_POINT('Ctrl Pts',(0.795684265985088,-0.190326085855194,
0.573915184558108));
#4861=CARTESIAN_POINT('Ctrl Pts',(0.813159949759,-0.15976606450048,0.548874290046456));
#4862=CARTESIAN_POINT('Ctrl Pts',(0.820511285096538,-0.142345102874864,
0.537715343527944));
#4863=CARTESIAN_POINT('Ctrl Pts',(0.833661031856294,-0.099930567888331,
0.517157748491653));
#4864=CARTESIAN_POINT('Ctrl Pts',(0.838633903678357,-0.0740444353928835,
0.508899795931835));
#4865=CARTESIAN_POINT('Ctrl Pts',(0.841298510752801,-0.0476299999999999,
0.504455939115715));
#4866=CARTESIAN_POINT('',(0.528110872004958,-0.04763,0.871530771444223));
#4867=CARTESIAN_POINT('Origin',(0.707106781186547,-0.04763,0.707106781186548));
#4868=CARTESIAN_POINT('',(0.871530771444223,-0.04763,0.528110872004959));
#4869=CARTESIAN_POINT('Ctrl Pts',(0.871530771444223,-0.0476300000000001,
0.528110872004958));
#4870=CARTESIAN_POINT('Ctrl Pts',(0.87014664509073,-0.0609922781173483,
0.530395067942936));
#4871=CARTESIAN_POINT('Ctrl Pts',(0.868149331745851,-0.0742967091364493,
0.533674141594226));
#4872=CARTESIAN_POINT('Ctrl Pts',(0.85981294420286,-0.115492077056649,0.54708917182331));
#4873=CARTESIAN_POINT('Ctrl Pts',(0.850993704737257,-0.141695629206859,
0.560922177770136));
#4874=CARTESIAN_POINT('Ctrl Pts',(0.830754510485543,-0.181890537957859,
0.590422647829571));
#4875=CARTESIAN_POINT('Ctrl Pts',(0.816896541396381,-0.201072148666545,
0.609616703125488));
#4876=CARTESIAN_POINT('Ctrl Pts',(0.792310597819928,-0.223955109275652,
0.641117951819998));
#4877=CARTESIAN_POINT('Ctrl Pts',(0.779109323683612,-0.232742381310829,
0.657208095763053));
#4878=CARTESIAN_POINT('Ctrl Pts',(0.750552691816206,-0.244234834628584,
0.68964083160521));
#4879=CARTESIAN_POINT('Ctrl Pts',(0.735185187071673,-0.246942143572133,
0.705971972091755));
#4880=CARTESIAN_POINT('Ctrl Pts',(0.705971972091754,-0.246942143572133,
0.735185187071673));
#4881=CARTESIAN_POINT('Ctrl Pts',(0.689640831605209,-0.244234834628584,
0.750552691816206));
#4882=CARTESIAN_POINT('Ctrl Pts',(0.657208095763052,-0.232742381310829,
0.779109323683612));
#4883=CARTESIAN_POINT('Ctrl Pts',(0.641117951819998,-0.223955109275652,
0.792310597819928));
#4884=CARTESIAN_POINT('Ctrl Pts',(0.609616703125487,-0.201072148666545,
0.816896541396382));
#4885=CARTESIAN_POINT('Ctrl Pts',(0.590422647829571,-0.181890537957858,
0.830754510485544));
#4886=CARTESIAN_POINT('Ctrl Pts',(0.560922177770135,-0.141695629206858,
0.850993704737257));
#4887=CARTESIAN_POINT('Ctrl Pts',(0.547089171823309,-0.115492077056649,
0.859812944202861));
#4888=CARTESIAN_POINT('Ctrl Pts',(0.533674141594226,-0.0742967091364491,
0.868149331745852));
#4889=CARTESIAN_POINT('Ctrl Pts',(0.530395067942936,-0.0609922781173483,
0.870146645090731));
#4890=CARTESIAN_POINT('Ctrl Pts',(0.528110872004958,-0.0476300000000001,
0.871530771444223));
#4891=CARTESIAN_POINT('Origin',(0.707106781186547,-0.04763,0.707106781186548));
#4892=CARTESIAN_POINT('Origin',(0.,-0.166705,0.));
#4893=CARTESIAN_POINT('',(0.242834539687906,-0.04763,0.989696097314));
#4894=CARTESIAN_POINT('Origin',(0.,-0.04763,0.));
#4895=CARTESIAN_POINT('',(-0.242834539687907,-0.04763,0.989696097314));
#4896=CARTESIAN_POINT('Ctrl Pts',(0.242834539687906,-0.04763,0.989696097314));
#4897=CARTESIAN_POINT('Ctrl Pts',(0.24024064412003,-0.0609922781173483,
0.990332542620729));
#4898=CARTESIAN_POINT('Ctrl Pts',(0.236509675094874,-0.0742967091364492,
0.991238884025248));
#4899=CARTESIAN_POINT('Ctrl Pts',(0.221129100087819,-0.115492077056649,
0.994830026707808));
#4900=CARTESIAN_POINT('Ctrl Pts',(0.205111543747588,-0.141695629206859,
0.998375294985966));
#4901=CARTESIAN_POINT('Ctrl Pts',(0.169940289819232,-0.181890537957859,
1.00492400591205));
#4902=CARTESIAN_POINT('Ctrl Pts',(0.1465689792446,-0.201072148666545,1.00869718865384));
#4903=CARTESIAN_POINT('Ctrl Pts',(0.106909345252087,-0.223955109275652,
1.01358704779679));
#4904=CARTESIAN_POINT('Ctrl Pts',(0.0861971848975941,-0.232742381310829,
1.0156297872271));
#4905=CARTESIAN_POINT('Ctrl Pts',(0.0430711894098822,-0.244234834628584,
1.01837060663223));
#4906=CARTESIAN_POINT('Ctrl Pts',(0.0206568624125605,-0.246942143572133,
1.019052));
#4907=CARTESIAN_POINT('Ctrl Pts',(-0.0206568624125608,-0.246942143572133,
1.019052));
#4908=CARTESIAN_POINT('Ctrl Pts',(-0.0430711894098825,-0.244234834628584,
1.01837060663223));
#4909=CARTESIAN_POINT('Ctrl Pts',(-0.0861971848975943,-0.232742381310829,
1.0156297872271));
#4910=CARTESIAN_POINT('Ctrl Pts',(-0.106909345252088,-0.223955109275652,
1.01358704779679));
#4911=CARTESIAN_POINT('Ctrl Pts',(-0.1465689792446,-0.201072148666545,1.00869718865384));
#4912=CARTESIAN_POINT('Ctrl Pts',(-0.169940289819232,-0.181890537957859,
1.00492400591205));
#4913=CARTESIAN_POINT('Ctrl Pts',(-0.205111543747588,-0.141695629206859,
0.998375294985966));
#4914=CARTESIAN_POINT('Ctrl Pts',(-0.221129100087819,-0.115492077056649,
0.994830026707808));
#4915=CARTESIAN_POINT('Ctrl Pts',(-0.236509675094875,-0.0742967091364493,
0.991238884025248));
#4916=CARTESIAN_POINT('Ctrl Pts',(-0.24024064412003,-0.0609922781173483,
0.990332542620729));
#4917=CARTESIAN_POINT('Ctrl Pts',(-0.242834539687907,-0.04763,0.989696097314));
#4918=CARTESIAN_POINT('',(-0.528110872004959,-0.04763,0.871530771444223));
#4919=CARTESIAN_POINT('Origin',(0.,-0.04763,0.));
#4920=CARTESIAN_POINT('',(-0.871530771444223,-0.04763,0.528110872004958));
#4921=CARTESIAN_POINT('Ctrl Pts',(-0.528110872004958,-0.0476300000000001,
0.871530771444223));
#4922=CARTESIAN_POINT('Ctrl Pts',(-0.530395067942936,-0.0609922781173484,
0.87014664509073));
#4923=CARTESIAN_POINT('Ctrl Pts',(-0.533674141594226,-0.0742967091364493,
0.868149331745851));
#4924=CARTESIAN_POINT('Ctrl Pts',(-0.54708917182331,-0.115492077056649,
0.85981294420286));
#4925=CARTESIAN_POINT('Ctrl Pts',(-0.560922177770136,-0.141695629206859,
0.850993704737257));
#4926=CARTESIAN_POINT('Ctrl Pts',(-0.590422647829571,-0.181890537957859,
0.830754510485543));
#4927=CARTESIAN_POINT('Ctrl Pts',(-0.609616703125488,-0.201072148666545,
0.816896541396381));
#4928=CARTESIAN_POINT('Ctrl Pts',(-0.641117951819998,-0.223955109275652,
0.792310597819928));
#4929=CARTESIAN_POINT('Ctrl Pts',(-0.657208095763053,-0.232742381310829,
0.779109323683611));
#4930=CARTESIAN_POINT('Ctrl Pts',(-0.68964083160521,-0.244234834628584,
0.750552691816205));
#4931=CARTESIAN_POINT('Ctrl Pts',(-0.705971972091755,-0.246942143572133,
0.735185187071673));
#4932=CARTESIAN_POINT('Ctrl Pts',(-0.735185187071673,-0.246942143572133,
0.705971972091754));
#4933=CARTESIAN_POINT('Ctrl Pts',(-0.750552691816206,-0.244234834628584,
0.689640831605209));
#4934=CARTESIAN_POINT('Ctrl Pts',(-0.779109323683612,-0.232742381310829,
0.657208095763052));
#4935=CARTESIAN_POINT('Ctrl Pts',(-0.792310597819928,-0.223955109275652,
0.641117951819998));
#4936=CARTESIAN_POINT('Ctrl Pts',(-0.816896541396382,-0.201072148666545,
0.609616703125487));
#4937=CARTESIAN_POINT('Ctrl Pts',(-0.830754510485544,-0.181890537957858,
0.590422647829571));
#4938=CARTESIAN_POINT('Ctrl Pts',(-0.850993704737257,-0.141695629206858,
0.560922177770135));
#4939=CARTESIAN_POINT('Ctrl Pts',(-0.859812944202861,-0.115492077056649,
0.547089171823309));
#4940=CARTESIAN_POINT('Ctrl Pts',(-0.868149331745852,-0.0742967091364491,
0.533674141594226));
#4941=CARTESIAN_POINT('Ctrl Pts',(-0.870146645090731,-0.0609922781173483,
0.530395067942936));
#4942=CARTESIAN_POINT('Ctrl Pts',(-0.871530771444223,-0.04763,0.528110872004958));
#4943=CARTESIAN_POINT('',(-0.989696097314,-0.04763,0.242834539687906));
#4944=CARTESIAN_POINT('Origin',(0.,-0.04763,0.));
#4945=CARTESIAN_POINT('',(-1.019052,-0.246942143572133,1.248489836334E-16));
#4946=CARTESIAN_POINT('Ctrl Pts',(-0.989696097314,-0.04763,0.242834539687906));
#4947=CARTESIAN_POINT('Ctrl Pts',(-0.990332542620729,-0.0609922781173483,
0.24024064412003));
#4948=CARTESIAN_POINT('Ctrl Pts',(-0.991238884025248,-0.0742967091364492,
0.236509675094874));
#4949=CARTESIAN_POINT('Ctrl Pts',(-0.994830026707808,-0.115492077056649,
0.221129100087819));
#4950=CARTESIAN_POINT('Ctrl Pts',(-0.998375294985966,-0.141695629206859,
0.205111543747588));
#4951=CARTESIAN_POINT('Ctrl Pts',(-1.00492400591205,-0.181890537957859,
0.169940289819232));
#4952=CARTESIAN_POINT('Ctrl Pts',(-1.00869718865384,-0.201072148666545,
0.1465689792446));
#4953=CARTESIAN_POINT('Ctrl Pts',(-1.01358704779679,-0.223955109275652,
0.106909345252088));
#4954=CARTESIAN_POINT('Ctrl Pts',(-1.0156297872271,-0.232742381310829,0.0861971848975944));
#4955=CARTESIAN_POINT('Ctrl Pts',(-1.01837060663223,-0.244234834628584,
0.0430711894098825));
#4956=CARTESIAN_POINT('Ctrl Pts',(-1.019052,-0.246942143572133,0.0206568624125608));
#4957=CARTESIAN_POINT('Ctrl Pts',(-1.019052,-0.246942143572133,1.2490009027033E-16));
#4958=CARTESIAN_POINT('',(-1.019052,-0.28578,1.24797876996471E-16));
#4959=CARTESIAN_POINT('',(-1.019052,-0.166705,1.24797876996471E-16));
#4960=CARTESIAN_POINT('Origin',(0.,-0.28578,0.));
#4961=CARTESIAN_POINT('',(-0.989696097314,-0.04763,-0.242834539687906));
#4962=CARTESIAN_POINT('Ctrl Pts',(-1.019052,-0.246942143572133,1.2490009027033E-16));
#4963=CARTESIAN_POINT('Ctrl Pts',(-1.019052,-0.246942143572133,-0.0206568624125605));
#4964=CARTESIAN_POINT('Ctrl Pts',(-1.01837060663223,-0.244234834628584,
-0.0430711894098822));
#4965=CARTESIAN_POINT('Ctrl Pts',(-1.0156297872271,-0.232742381310829,-0.0861971848975941));
#4966=CARTESIAN_POINT('Ctrl Pts',(-1.01358704779679,-0.223955109275652,
-0.106909345252087));
#4967=CARTESIAN_POINT('Ctrl Pts',(-1.00869718865384,-0.201072148666546,
-0.1465689792446));
#4968=CARTESIAN_POINT('Ctrl Pts',(-1.00492400591205,-0.181890537957859,
-0.169940289819232));
#4969=CARTESIAN_POINT('Ctrl Pts',(-0.998375294985966,-0.141695629206859,
-0.205111543747588));
#4970=CARTESIAN_POINT('Ctrl Pts',(-0.994830026707808,-0.11549207705665,
-0.221129100087819));
#4971=CARTESIAN_POINT('Ctrl Pts',(-0.991238884025248,-0.0742967091364495,
-0.236509675094874));
#4972=CARTESIAN_POINT('Ctrl Pts',(-0.990332542620729,-0.0609922781173484,
-0.24024064412003));
#4973=CARTESIAN_POINT('Ctrl Pts',(-0.989696097314,-0.0476300000000001,-0.242834539687907));
#4974=CARTESIAN_POINT('',(-0.871530771444223,-0.04763,-0.528110872004958));
#4975=CARTESIAN_POINT('Origin',(0.,-0.04763,0.));
#4976=CARTESIAN_POINT('',(-0.528110872004958,-0.04763,-0.871530771444223));
#4977=CARTESIAN_POINT('Ctrl Pts',(-0.871530771444223,-0.0476300000000001,
-0.528110872004958));
#4978=CARTESIAN_POINT('Ctrl Pts',(-0.87014664509073,-0.0609922781173484,
-0.530395067942936));
#4979=CARTESIAN_POINT('Ctrl Pts',(-0.868149331745851,-0.0742967091364494,
-0.533674141594226));
#4980=CARTESIAN_POINT('Ctrl Pts',(-0.85981294420286,-0.115492077056649,
-0.54708917182331));
#4981=CARTESIAN_POINT('Ctrl Pts',(-0.850993704737257,-0.141695629206859,
-0.560922177770136));
#4982=CARTESIAN_POINT('Ctrl Pts',(-0.830754510485543,-0.181890537957859,
-0.590422647829571));
#4983=CARTESIAN_POINT('Ctrl Pts',(-0.816896541396381,-0.201072148666546,
-0.609616703125488));
#4984=CARTESIAN_POINT('Ctrl Pts',(-0.792310597819928,-0.223955109275652,
-0.641117951819999));
#4985=CARTESIAN_POINT('Ctrl Pts',(-0.779109323683611,-0.232742381310829,
-0.657208095763053));
#4986=CARTESIAN_POINT('Ctrl Pts',(-0.750552691816205,-0.244234834628584,
-0.68964083160521));
#4987=CARTESIAN_POINT('Ctrl Pts',(-0.735185187071673,-0.246942143572133,
-0.705971972091755));
#4988=CARTESIAN_POINT('Ctrl Pts',(-0.705971972091754,-0.246942143572133,
-0.735185187071673));
#4989=CARTESIAN_POINT('Ctrl Pts',(-0.68964083160521,-0.244234834628584,
-0.750552691816206));
#4990=CARTESIAN_POINT('Ctrl Pts',(-0.657208095763052,-0.232742381310829,
-0.779109323683612));
#4991=CARTESIAN_POINT('Ctrl Pts',(-0.641117951819998,-0.223955109275652,
-0.792310597819928));
#4992=CARTESIAN_POINT('Ctrl Pts',(-0.609616703125488,-0.201072148666545,
-0.816896541396381));
#4993=CARTESIAN_POINT('Ctrl Pts',(-0.590422647829571,-0.181890537957859,
-0.830754510485543));
#4994=CARTESIAN_POINT('Ctrl Pts',(-0.560922177770136,-0.141695629206859,
-0.850993704737257));
#4995=CARTESIAN_POINT('Ctrl Pts',(-0.54708917182331,-0.115492077056649,
-0.85981294420286));
#4996=CARTESIAN_POINT('Ctrl Pts',(-0.533674141594226,-0.0742967091364494,
-0.868149331745852));
#4997=CARTESIAN_POINT('Ctrl Pts',(-0.530395067942936,-0.0609922781173484,
-0.870146645090731));
#4998=CARTESIAN_POINT('Ctrl Pts',(-0.528110872004958,-0.0476300000000001,
-0.871530771444223));
#4999=CARTESIAN_POINT('',(-0.242834539687906,-0.04763,-0.989696097314));
#5000=CARTESIAN_POINT('Origin',(0.,-0.04763,0.));
#5001=CARTESIAN_POINT('',(0.242834539687906,-0.04763,-0.989696097314));
#5002=CARTESIAN_POINT('Ctrl Pts',(-0.242834539687907,-0.04763,-0.989696097314));
#5003=CARTESIAN_POINT('Ctrl Pts',(-0.24024064412003,-0.0609922781173483,
-0.990332542620729));
#5004=CARTESIAN_POINT('Ctrl Pts',(-0.236509675094874,-0.0742967091364493,
-0.991238884025248));
#5005=CARTESIAN_POINT('Ctrl Pts',(-0.221129100087819,-0.115492077056649,
-0.994830026707808));
#5006=CARTESIAN_POINT('Ctrl Pts',(-0.205111543747588,-0.141695629206859,
-0.998375294985966));
#5007=CARTESIAN_POINT('Ctrl Pts',(-0.169940289819232,-0.181890537957859,
-1.00492400591205));
#5008=CARTESIAN_POINT('Ctrl Pts',(-0.1465689792446,-0.201072148666545,-1.00869718865384));
#5009=CARTESIAN_POINT('Ctrl Pts',(-0.106909345252087,-0.223955109275652,
-1.01358704779679));
#5010=CARTESIAN_POINT('Ctrl Pts',(-0.0861971848975942,-0.232742381310829,
-1.0156297872271));
#5011=CARTESIAN_POINT('Ctrl Pts',(-0.0430711894098823,-0.244234834628584,
-1.01837060663223));
#5012=CARTESIAN_POINT('Ctrl Pts',(-0.0206568624125606,-0.246942143572133,
-1.019052));
#5013=CARTESIAN_POINT('Ctrl Pts',(0.0206568624125607,-0.246942143572133,
-1.019052));
#5014=CARTESIAN_POINT('Ctrl Pts',(0.0430711894098824,-0.244234834628584,
-1.01837060663223));
#5015=CARTESIAN_POINT('Ctrl Pts',(0.0861971848975943,-0.232742381310829,
-1.0156297872271));
#5016=CARTESIAN_POINT('Ctrl Pts',(0.106909345252088,-0.223955109275652,
-1.01358704779679));
#5017=CARTESIAN_POINT('Ctrl Pts',(0.1465689792446,-0.201072148666545,-1.00869718865384));
#5018=CARTESIAN_POINT('Ctrl Pts',(0.169940289819232,-0.181890537957859,
-1.00492400591205));
#5019=CARTESIAN_POINT('Ctrl Pts',(0.205111543747588,-0.141695629206859,
-0.998375294985966));
#5020=CARTESIAN_POINT('Ctrl Pts',(0.221129100087819,-0.115492077056649,
-0.994830026707808));
#5021=CARTESIAN_POINT('Ctrl Pts',(0.236509675094874,-0.0742967091364493,
-0.991238884025248));
#5022=CARTESIAN_POINT('Ctrl Pts',(0.24024064412003,-0.0609922781173484,
-0.990332542620729));
#5023=CARTESIAN_POINT('Ctrl Pts',(0.242834539687907,-0.04763,-0.989696097314));
#5024=CARTESIAN_POINT('',(0.528110872004958,-0.04763,-0.871530771444223));
#5025=CARTESIAN_POINT('Origin',(0.,-0.04763,0.));
#5026=CARTESIAN_POINT('',(0.871530771444223,-0.04763,-0.528110872004958));
#5027=CARTESIAN_POINT('Ctrl Pts',(0.528110872004958,-0.0476300000000001,
-0.871530771444223));
#5028=CARTESIAN_POINT('Ctrl Pts',(0.530395067942936,-0.0609922781173484,
-0.870146645090731));
#5029=CARTESIAN_POINT('Ctrl Pts',(0.533674141594226,-0.0742967091364493,
-0.868149331745851));
#5030=CARTESIAN_POINT('Ctrl Pts',(0.54708917182331,-0.115492077056649,-0.85981294420286));
#5031=CARTESIAN_POINT('Ctrl Pts',(0.560922177770136,-0.141695629206859,
-0.850993704737257));
#5032=CARTESIAN_POINT('Ctrl Pts',(0.590422647829571,-0.181890537957859,
-0.830754510485543));
#5033=CARTESIAN_POINT('Ctrl Pts',(0.609616703125488,-0.201072148666545,
-0.816896541396381));
#5034=CARTESIAN_POINT('Ctrl Pts',(0.641117951819998,-0.223955109275652,
-0.792310597819928));
#5035=CARTESIAN_POINT('Ctrl Pts',(0.657208095763053,-0.232742381310829,
-0.779109323683612));
#5036=CARTESIAN_POINT('Ctrl Pts',(0.68964083160521,-0.244234834628584,-0.750552691816206));
#5037=CARTESIAN_POINT('Ctrl Pts',(0.705971972091755,-0.246942143572133,
-0.735185187071673));
#5038=CARTESIAN_POINT('Ctrl Pts',(0.735185187071673,-0.246942143572133,
-0.705971972091754));
#5039=CARTESIAN_POINT('Ctrl Pts',(0.750552691816206,-0.244234834628584,
-0.68964083160521));
#5040=CARTESIAN_POINT('Ctrl Pts',(0.779109323683612,-0.232742381310829,
-0.657208095763053));
#5041=CARTESIAN_POINT('Ctrl Pts',(0.792310597819928,-0.223955109275652,
-0.641117951819998));
#5042=CARTESIAN_POINT('Ctrl Pts',(0.816896541396381,-0.201072148666545,
-0.609616703125488));
#5043=CARTESIAN_POINT('Ctrl Pts',(0.830754510485543,-0.181890537957859,
-0.590422647829571));
#5044=CARTESIAN_POINT('Ctrl Pts',(0.850993704737257,-0.141695629206859,
-0.560922177770136));
#5045=CARTESIAN_POINT('Ctrl Pts',(0.85981294420286,-0.115492077056649,-0.54708917182331));
#5046=CARTESIAN_POINT('Ctrl Pts',(0.868149331745851,-0.0742967091364493,
-0.533674141594226));
#5047=CARTESIAN_POINT('Ctrl Pts',(0.870146645090731,-0.0609922781173484,
-0.530395067942936));
#5048=CARTESIAN_POINT('Ctrl Pts',(0.871530771444223,-0.0476300000000001,
-0.528110872004958));
#5049=CARTESIAN_POINT('',(0.989696097314,-0.04763,-0.242834539687906));
#5050=CARTESIAN_POINT('Origin',(0.,-0.04763,0.));
#5051=CARTESIAN_POINT('',(0.989696097314,-0.04763,0.242834539687906));
#5052=CARTESIAN_POINT('Ctrl Pts',(0.989696097314,-0.04763,-0.242834539687907));
#5053=CARTESIAN_POINT('Ctrl Pts',(0.990332542620729,-0.0609922781173483,
-0.24024064412003));
#5054=CARTESIAN_POINT('Ctrl Pts',(0.991238884025248,-0.0742967091364493,
-0.236509675094874));
#5055=CARTESIAN_POINT('Ctrl Pts',(0.994830026707808,-0.115492077056649,
-0.221129100087819));
#5056=CARTESIAN_POINT('Ctrl Pts',(0.998375294985966,-0.141695629206859,
-0.205111543747588));
#5057=CARTESIAN_POINT('Ctrl Pts',(1.00492400591205,-0.181890537957859,-0.169940289819232));
#5058=CARTESIAN_POINT('Ctrl Pts',(1.00869718865384,-0.201072148666545,-0.1465689792446));
#5059=CARTESIAN_POINT('Ctrl Pts',(1.01358704779679,-0.223955109275652,-0.106909345252087));
#5060=CARTESIAN_POINT('Ctrl Pts',(1.0156297872271,-0.232742381310829,-0.0861971848975942));
#5061=CARTESIAN_POINT('Ctrl Pts',(1.01837060663223,-0.244234834628584,-0.0430711894098823));
#5062=CARTESIAN_POINT('Ctrl Pts',(1.019052,-0.246942143572133,-0.0206568624125607));
#5063=CARTESIAN_POINT('Ctrl Pts',(1.019052,-0.246942143572133,0.0206568624125607));
#5064=CARTESIAN_POINT('Ctrl Pts',(1.01837060663223,-0.244234834628584,0.0430711894098823));
#5065=CARTESIAN_POINT('Ctrl Pts',(1.0156297872271,-0.232742381310829,0.0861971848975942));
#5066=CARTESIAN_POINT('Ctrl Pts',(1.01358704779679,-0.223955109275652,0.106909345252087));
#5067=CARTESIAN_POINT('Ctrl Pts',(1.00869718865384,-0.201072148666545,0.1465689792446));
#5068=CARTESIAN_POINT('Ctrl Pts',(1.00492400591205,-0.181890537957859,0.169940289819232));
#5069=CARTESIAN_POINT('Ctrl Pts',(0.998375294985966,-0.141695629206859,
0.205111543747588));
#5070=CARTESIAN_POINT('Ctrl Pts',(0.994830026707808,-0.115492077056649,
0.221129100087819));
#5071=CARTESIAN_POINT('Ctrl Pts',(0.991238884025248,-0.0742967091364492,
0.236509675094874));
#5072=CARTESIAN_POINT('Ctrl Pts',(0.990332542620729,-0.0609922781173483,
0.24024064412003));
#5073=CARTESIAN_POINT('Ctrl Pts',(0.989696097314,-0.04763,0.242834539687907));
#5074=CARTESIAN_POINT('Origin',(0.,-0.04763,0.));
#5075=CARTESIAN_POINT('Origin',(0.,-0.04763,0.));
#5076=CARTESIAN_POINT('',(0.238183666596899,-0.04763,0.951592097314));
#5077=CARTESIAN_POINT('Origin',(0.,-0.04763,0.));
#5078=CARTESIAN_POINT('Origin',(-1.94289029309402E-16,-0.04763,1.));
#5079=CARTESIAN_POINT('Origin',(-1.94289029309402E-16,0.,1.));
#5080=CARTESIAN_POINT('',(-0.2381836665969,-0.04763,0.951592097314));
#5081=CARTESIAN_POINT('Ctrl Pts',(-0.238183666596899,-0.0476299999999999,
0.951592097314));
#5082=CARTESIAN_POINT('Ctrl Pts',(-0.233157223576062,-0.0740444353928835,
0.952850216871763));
#5083=CARTESIAN_POINT('Ctrl Pts',(-0.223801617934946,-0.0999305678883309,
0.955173119738174));
#5084=CARTESIAN_POINT('Ctrl Pts',(-0.199966927975188,-0.142345102874864,
0.960411259488514));
#5085=CARTESIAN_POINT('Ctrl Pts',(-0.1868781821531,-0.159766064500479,0.963103647174702));
#5086=CARTESIAN_POINT('Ctrl Pts',(-0.15681442133453,-0.190326085855194,
0.968453058988463));
#5087=CARTESIAN_POINT('Ctrl Pts',(-0.139836317888043,-0.203463743702801,
0.971100730005489));
#5088=CARTESIAN_POINT('Ctrl Pts',(-0.104422493053067,-0.224161999508995,
0.975530745318961));
#5089=CARTESIAN_POINT('Ctrl Pts',(-0.0842175114474176,-0.232861760990032,
0.977553872336861));
#5090=CARTESIAN_POINT('Ctrl Pts',(-0.0421062857595701,-0.244251601209411,
0.980270995488453));
#5091=CARTESIAN_POINT('Ctrl Pts',(-0.0201990724523197,-0.246942143572133,
0.980948));
#5092=CARTESIAN_POINT('Ctrl Pts',(0.020199072452319,-0.246942143572133,
0.980948));
#5093=CARTESIAN_POINT('Ctrl Pts',(0.0421062857595694,-0.244251601209411,
0.980270995488454));
#5094=CARTESIAN_POINT('Ctrl Pts',(0.0842175114474169,-0.232861760990032,
0.977553872336861));
#5095=CARTESIAN_POINT('Ctrl Pts',(0.104422493053067,-0.224161999508995,
0.975530745318961));
#5096=CARTESIAN_POINT('Ctrl Pts',(0.139836317888042,-0.203463743702801,
0.971100730005489));
#5097=CARTESIAN_POINT('Ctrl Pts',(0.15681442133453,-0.190326085855194,0.968453058988463));
#5098=CARTESIAN_POINT('Ctrl Pts',(0.1868781821531,-0.15976606450048,0.963103647174702));
#5099=CARTESIAN_POINT('Ctrl Pts',(0.199966927975188,-0.142345102874864,
0.960411259488514));
#5100=CARTESIAN_POINT('Ctrl Pts',(0.223801617934945,-0.0999305678883309,
0.955173119738174));
#5101=CARTESIAN_POINT('Ctrl Pts',(0.233157223576061,-0.0740444353928835,
0.952850216871763));
#5102=CARTESIAN_POINT('Ctrl Pts',(0.238183666596899,-0.0476299999999999,
0.951592097314));
#5103=CARTESIAN_POINT('Origin',(-1.94289029309402E-16,-0.04763,1.));
#5104=CARTESIAN_POINT('Origin',(0.,-0.04763,0.));
#5105=CARTESIAN_POINT('',(-0.504455939115715,-0.04763,0.841298510752802));
#5106=CARTESIAN_POINT('Origin',(0.,-0.04763,0.));
#5107=CARTESIAN_POINT('Origin',(-0.707106781186548,-0.04763,0.707106781186547));
#5108=CARTESIAN_POINT('Origin',(-0.707106781186548,0.,0.707106781186547));
#5109=CARTESIAN_POINT('',(-0.841298510752802,-0.04763,0.504455939115715));
#5110=CARTESIAN_POINT('Ctrl Pts',(-0.841298510752802,-0.04763,0.504455939115715));
#5111=CARTESIAN_POINT('Ctrl Pts',(-0.838633903678357,-0.0740444353928835,
0.508899795931835));
#5112=CARTESIAN_POINT('Ctrl Pts',(-0.833661031856294,-0.0999305678883309,
0.517157748491652));
#5113=CARTESIAN_POINT('Ctrl Pts',(-0.820511285096538,-0.142345102874864,
0.537715343527944));
#5114=CARTESIAN_POINT('Ctrl Pts',(-0.813159949759,-0.159766064500479,0.548874290046456));
#5115=CARTESIAN_POINT('Ctrl Pts',(-0.795684265985089,-0.190326085855194,
0.573915184558107));
#5116=CARTESIAN_POINT('Ctrl Pts',(-0.78555112003688,-0.203463743702801,
0.587792702767295));
#5117=CARTESIAN_POINT('Ctrl Pts',(-0.763642258217233,-0.224161999508995,
0.615966552324775));
#5118=CARTESIAN_POINT('Ctrl Pts',(-0.750785745543687,-0.232861760990032,
0.631684198665438));
#5119=CARTESIAN_POINT('Ctrl Pts',(-0.722929908501543,-0.244251601209411,
0.663382628119203));
#5120=CARTESIAN_POINT('Ctrl Pts',(-0.707917883896095,-0.246942143572133,
0.679352081686668));
#5121=CARTESIAN_POINT('Ctrl Pts',(-0.679352081686668,-0.246942143572133,
0.707917883896095));
#5122=CARTESIAN_POINT('Ctrl Pts',(-0.663382628119203,-0.244251601209411,
0.722929908501544));
#5123=CARTESIAN_POINT('Ctrl Pts',(-0.631684198665438,-0.232861760990031,
0.750785745543687));
#5124=CARTESIAN_POINT('Ctrl Pts',(-0.615966552324775,-0.224161999508995,
0.763642258217233));
#5125=CARTESIAN_POINT('Ctrl Pts',(-0.587792702767295,-0.203463743702801,
0.78555112003688));
#5126=CARTESIAN_POINT('Ctrl Pts',(-0.573915184558107,-0.190326085855194,
0.795684265985088));
#5127=CARTESIAN_POINT('Ctrl Pts',(-0.548874290046456,-0.159766064500479,
0.813159949759));
#5128=CARTESIAN_POINT('Ctrl Pts',(-0.537715343527944,-0.142345102874864,
0.820511285096538));
#5129=CARTESIAN_POINT('Ctrl Pts',(-0.517157748491652,-0.0999305678883309,
0.833661031856294));
#5130=CARTESIAN_POINT('Ctrl Pts',(-0.508899795931835,-0.0740444353928835,
0.838633903678357));
#5131=CARTESIAN_POINT('Ctrl Pts',(-0.504455939115716,-0.04763,0.841298510752801));
#5132=CARTESIAN_POINT('Origin',(-0.707106781186548,-0.04763,0.707106781186547));
#5133=CARTESIAN_POINT('Origin',(0.,-0.04763,0.));
#5134=CARTESIAN_POINT('',(-0.951592097314,-0.04763,0.238183666596899));
#5135=CARTESIAN_POINT('Origin',(0.,-0.04763,0.));
#5136=CARTESIAN_POINT('Origin',(-1.,-0.04763,-1.11022302462516E-16));
#5137=CARTESIAN_POINT('Origin',(-1.,0.,-1.11022302462516E-16));
#5138=CARTESIAN_POINT('',(-0.951592097314,-0.04763,-0.2381836665969));
#5139=CARTESIAN_POINT('',(-0.980948,-0.246942143572133,1.08514323328844E-18));
#5140=CARTESIAN_POINT('Ctrl Pts',(-0.951592097314,-0.04763,-0.238183666596899));
#5141=CARTESIAN_POINT('Ctrl Pts',(-0.952850216871763,-0.0740444353928835,
-0.233157223576062));
#5142=CARTESIAN_POINT('Ctrl Pts',(-0.955173119738174,-0.0999305678883309,
-0.223801617934946));
#5143=CARTESIAN_POINT('Ctrl Pts',(-0.960411259488514,-0.142345102874864,
-0.199966927975188));
#5144=CARTESIAN_POINT('Ctrl Pts',(-0.963103647174702,-0.159766064500479,
-0.1868781821531));
#5145=CARTESIAN_POINT('Ctrl Pts',(-0.968453058988463,-0.190326085855194,
-0.15681442133453));
#5146=CARTESIAN_POINT('Ctrl Pts',(-0.971100730005489,-0.203463743702801,
-0.139836317888043));
#5147=CARTESIAN_POINT('Ctrl Pts',(-0.975530745318961,-0.224161999508995,
-0.104422493053067));
#5148=CARTESIAN_POINT('Ctrl Pts',(-0.977553872336861,-0.232861760990032,
-0.0842175114474175));
#5149=CARTESIAN_POINT('Ctrl Pts',(-0.980270995488453,-0.244251601209411,
-0.0421062857595699));
#5150=CARTESIAN_POINT('Ctrl Pts',(-0.980948,-0.246942143572133,-0.0201990724523195));
#5151=CARTESIAN_POINT('Ctrl Pts',(-0.980948,-0.246942143572133,-1.17961196366423E-16));
#5152=CARTESIAN_POINT('Origin',(-1.,-0.04763,-1.11022302462516E-16));
#5153=CARTESIAN_POINT('Ctrl Pts',(-0.980948,-0.246942143572133,-1.17961196366423E-16));
#5154=CARTESIAN_POINT('Ctrl Pts',(-0.980948,-0.246942143572133,0.0201990724523192));
#5155=CARTESIAN_POINT('Ctrl Pts',(-0.980270995488453,-0.244251601209411,
0.0421062857595695));
#5156=CARTESIAN_POINT('Ctrl Pts',(-0.977553872336861,-0.232861760990032,
0.0842175114474169));
#5157=CARTESIAN_POINT('Ctrl Pts',(-0.975530745318961,-0.224161999508995,
0.104422493053066));
#5158=CARTESIAN_POINT('Ctrl Pts',(-0.971100730005489,-0.203463743702801,
0.139836317888042));
#5159=CARTESIAN_POINT('Ctrl Pts',(-0.968453058988463,-0.190326085855194,
0.15681442133453));
#5160=CARTESIAN_POINT('Ctrl Pts',(-0.963103647174702,-0.15976606450048,
0.1868781821531));
#5161=CARTESIAN_POINT('Ctrl Pts',(-0.960411259488514,-0.142345102874864,
0.199966927975188));
#5162=CARTESIAN_POINT('Ctrl Pts',(-0.955173119738174,-0.099930567888331,
0.223801617934945));
#5163=CARTESIAN_POINT('Ctrl Pts',(-0.952850216871763,-0.0740444353928835,
0.233157223576061));
#5164=CARTESIAN_POINT('Ctrl Pts',(-0.951592097314,-0.04763,0.238183666596899));
#5165=CARTESIAN_POINT('Origin',(0.,-0.04763,0.));
#5166=CARTESIAN_POINT('',(-0.841298510752802,-0.04763,-0.504455939115715));
#5167=CARTESIAN_POINT('Origin',(0.,-0.04763,0.));
#5168=CARTESIAN_POINT('Origin',(-0.707106781186547,-0.04763,-0.707106781186548));
#5169=CARTESIAN_POINT('Origin',(-0.707106781186547,0.,-0.707106781186548));
#5170=CARTESIAN_POINT('',(-0.504455939115715,-0.04763,-0.841298510752802));
#5171=CARTESIAN_POINT('Ctrl Pts',(-0.504455939115715,-0.04763,-0.841298510752802));
#5172=CARTESIAN_POINT('Ctrl Pts',(-0.508899795931835,-0.0740444353928835,
-0.838633903678357));
#5173=CARTESIAN_POINT('Ctrl Pts',(-0.517157748491652,-0.0999305678883309,
-0.833661031856294));
#5174=CARTESIAN_POINT('Ctrl Pts',(-0.537715343527944,-0.142345102874864,
-0.820511285096538));
#5175=CARTESIAN_POINT('Ctrl Pts',(-0.548874290046456,-0.159766064500479,
-0.813159949759));
#5176=CARTESIAN_POINT('Ctrl Pts',(-0.573915184558107,-0.190326085855194,
-0.795684265985089));
#5177=CARTESIAN_POINT('Ctrl Pts',(-0.587792702767295,-0.203463743702801,
-0.78555112003688));
#5178=CARTESIAN_POINT('Ctrl Pts',(-0.615966552324775,-0.224161999508995,
-0.763642258217233));
#5179=CARTESIAN_POINT('Ctrl Pts',(-0.631684198665438,-0.232861760990032,
-0.750785745543687));
#5180=CARTESIAN_POINT('Ctrl Pts',(-0.663382628119203,-0.244251601209411,
-0.722929908501543));
#5181=CARTESIAN_POINT('Ctrl Pts',(-0.679352081686668,-0.246942143572133,
-0.707917883896095));
#5182=CARTESIAN_POINT('Ctrl Pts',(-0.707917883896095,-0.246942143572133,
-0.679352081686668));
#5183=CARTESIAN_POINT('Ctrl Pts',(-0.722929908501543,-0.244251601209411,
-0.663382628119203));
#5184=CARTESIAN_POINT('Ctrl Pts',(-0.750785745543687,-0.232861760990032,
-0.631684198665439));
#5185=CARTESIAN_POINT('Ctrl Pts',(-0.763642258217232,-0.224161999508995,
-0.615966552324775));
#5186=CARTESIAN_POINT('Ctrl Pts',(-0.78555112003688,-0.203463743702801,
-0.587792702767295));
#5187=CARTESIAN_POINT('Ctrl Pts',(-0.795684265985088,-0.190326085855194,
-0.573915184558107));
#5188=CARTESIAN_POINT('Ctrl Pts',(-0.813159949759,-0.15976606450048,-0.548874290046456));
#5189=CARTESIAN_POINT('Ctrl Pts',(-0.820511285096538,-0.142345102874864,
-0.537715343527944));
#5190=CARTESIAN_POINT('Ctrl Pts',(-0.833661031856294,-0.0999305678883311,
-0.517157748491652));
#5191=CARTESIAN_POINT('Ctrl Pts',(-0.838633903678357,-0.0740444353928836,
-0.508899795931835));
#5192=CARTESIAN_POINT('Ctrl Pts',(-0.841298510752801,-0.04763,-0.504455939115715));
#5193=CARTESIAN_POINT('Origin',(-0.707106781186547,-0.04763,-0.707106781186548));
#5194=CARTESIAN_POINT('Origin',(0.,-0.04763,0.));
#5195=CARTESIAN_POINT('',(-0.238183666596899,-0.04763,-0.951592097314));
#5196=CARTESIAN_POINT('Origin',(0.,-0.04763,0.));
#5197=CARTESIAN_POINT('Origin',(5.55111512312578E-17,-0.04763,-1.));
#5198=CARTESIAN_POINT('Origin',(5.55111512312578E-17,0.,-1.));
#5199=CARTESIAN_POINT('',(0.238183666596899,-0.04763,-0.951592097314));
#5200=CARTESIAN_POINT('Ctrl Pts',(0.238183666596899,-0.04763,-0.951592097314));
#5201=CARTESIAN_POINT('Ctrl Pts',(0.233157223576062,-0.0740444353928835,
-0.952850216871763));
#5202=CARTESIAN_POINT('Ctrl Pts',(0.223801617934946,-0.099930567888331,
-0.955173119738174));
#5203=CARTESIAN_POINT('Ctrl Pts',(0.199966927975188,-0.142345102874864,
-0.960411259488514));
#5204=CARTESIAN_POINT('Ctrl Pts',(0.1868781821531,-0.15976606450048,-0.963103647174702));
#5205=CARTESIAN_POINT('Ctrl Pts',(0.15681442133453,-0.190326085855194,-0.968453058988463));
#5206=CARTESIAN_POINT('Ctrl Pts',(0.139836317888042,-0.203463743702801,
-0.971100730005489));
#5207=CARTESIAN_POINT('Ctrl Pts',(0.104422493053067,-0.224161999508995,
-0.975530745318961));
#5208=CARTESIAN_POINT('Ctrl Pts',(0.0842175114474173,-0.232861760990032,
-0.977553872336861));
#5209=CARTESIAN_POINT('Ctrl Pts',(0.0421062857595698,-0.244251601209411,
-0.980270995488453));
#5210=CARTESIAN_POINT('Ctrl Pts',(0.0201990724523194,-0.246942143572133,
-0.980948));
#5211=CARTESIAN_POINT('Ctrl Pts',(-0.0201990724523193,-0.246942143572133,
-0.980948));
#5212=CARTESIAN_POINT('Ctrl Pts',(-0.0421062857595697,-0.244251601209411,
-0.980270995488453));
#5213=CARTESIAN_POINT('Ctrl Pts',(-0.0842175114474171,-0.232861760990032,
-0.977553872336861));
#5214=CARTESIAN_POINT('Ctrl Pts',(-0.104422493053067,-0.224161999508995,
-0.975530745318961));
#5215=CARTESIAN_POINT('Ctrl Pts',(-0.139836317888042,-0.203463743702801,
-0.971100730005489));
#5216=CARTESIAN_POINT('Ctrl Pts',(-0.15681442133453,-0.190326085855194,
-0.968453058988463));
#5217=CARTESIAN_POINT('Ctrl Pts',(-0.1868781821531,-0.15976606450048,-0.963103647174702));
#5218=CARTESIAN_POINT('Ctrl Pts',(-0.199966927975188,-0.142345102874864,
-0.960411259488514));
#5219=CARTESIAN_POINT('Ctrl Pts',(-0.223801617934945,-0.099930567888331,
-0.955173119738174));
#5220=CARTESIAN_POINT('Ctrl Pts',(-0.233157223576062,-0.0740444353928835,
-0.952850216871763));
#5221=CARTESIAN_POINT('Ctrl Pts',(-0.238183666596899,-0.0476299999999999,
-0.951592097314));
#5222=CARTESIAN_POINT('Origin',(5.55111512312578E-17,-0.04763,-1.));
#5223=CARTESIAN_POINT('Origin',(0.,-0.04763,0.));
#5224=CARTESIAN_POINT('',(0.504455939115715,-0.04763,-0.841298510752802));
#5225=CARTESIAN_POINT('Origin',(0.,-0.04763,0.));
#5226=CARTESIAN_POINT('Origin',(0.707106781186548,-0.04763,-0.707106781186547));
#5227=CARTESIAN_POINT('Origin',(0.707106781186548,0.,-0.707106781186547));
#5228=CARTESIAN_POINT('',(0.841298510752802,-0.04763,-0.504455939115715));
#5229=CARTESIAN_POINT('Ctrl Pts',(0.841298510752802,-0.04763,-0.504455939115715));
#5230=CARTESIAN_POINT('Ctrl Pts',(0.838633903678357,-0.0740444353928835,
-0.508899795931835));
#5231=CARTESIAN_POINT('Ctrl Pts',(0.833661031856294,-0.0999305678883309,
-0.517157748491652));
#5232=CARTESIAN_POINT('Ctrl Pts',(0.820511285096538,-0.142345102874864,
-0.537715343527944));
#5233=CARTESIAN_POINT('Ctrl Pts',(0.813159949759,-0.159766064500479,-0.548874290046456));
#5234=CARTESIAN_POINT('Ctrl Pts',(0.795684265985088,-0.190326085855194,
-0.573915184558107));
#5235=CARTESIAN_POINT('Ctrl Pts',(0.78555112003688,-0.203463743702801,-0.587792702767295));
#5236=CARTESIAN_POINT('Ctrl Pts',(0.763642258217233,-0.224161999508995,
-0.615966552324775));
#5237=CARTESIAN_POINT('Ctrl Pts',(0.750785745543687,-0.232861760990032,
-0.631684198665438));
#5238=CARTESIAN_POINT('Ctrl Pts',(0.722929908501543,-0.244251601209411,
-0.663382628119203));
#5239=CARTESIAN_POINT('Ctrl Pts',(0.707917883896095,-0.246942143572133,
-0.679352081686668));
#5240=CARTESIAN_POINT('Ctrl Pts',(0.679352081686668,-0.246942143572133,
-0.707917883896095));
#5241=CARTESIAN_POINT('Ctrl Pts',(0.663382628119203,-0.244251601209411,
-0.722929908501543));
#5242=CARTESIAN_POINT('Ctrl Pts',(0.631684198665438,-0.232861760990032,
-0.750785745543687));
#5243=CARTESIAN_POINT('Ctrl Pts',(0.615966552324775,-0.224161999508995,
-0.763642258217232));
#5244=CARTESIAN_POINT('Ctrl Pts',(0.587792702767295,-0.203463743702801,
-0.78555112003688));
#5245=CARTESIAN_POINT('Ctrl Pts',(0.573915184558107,-0.190326085855194,
-0.795684265985088));
#5246=CARTESIAN_POINT('Ctrl Pts',(0.548874290046456,-0.159766064500479,
-0.813159949759));
#5247=CARTESIAN_POINT('Ctrl Pts',(0.537715343527944,-0.142345102874864,
-0.820511285096538));
#5248=CARTESIAN_POINT('Ctrl Pts',(0.517157748491652,-0.099930567888331,
-0.833661031856294));
#5249=CARTESIAN_POINT('Ctrl Pts',(0.508899795931835,-0.0740444353928835,
-0.838633903678357));
#5250=CARTESIAN_POINT('Ctrl Pts',(0.504455939115715,-0.04763,-0.841298510752801));
#5251=CARTESIAN_POINT('Origin',(0.707106781186548,-0.04763,-0.707106781186547));
#5252=CARTESIAN_POINT('Origin',(0.,-0.166705,0.));
#5253=CARTESIAN_POINT('',(-0.980948,-0.28578,1.20131482833E-16));
#5254=CARTESIAN_POINT('Origin',(0.,-0.28578,0.));
#5255=CARTESIAN_POINT('',(-0.980948,-0.166705,1.20131482833E-16));
#5256=CARTESIAN_POINT('',(0.951592097314,-0.04763,0.238183666596899));
#5257=CARTESIAN_POINT('Origin',(0.,-0.04763,0.));
#5258=CARTESIAN_POINT('',(0.951592097314,-0.04763,-0.238183666596899));
#5259=CARTESIAN_POINT('Ctrl Pts',(0.951592097314,-0.04763,0.238183666596899));
#5260=CARTESIAN_POINT('Ctrl Pts',(0.952850216871763,-0.0740444353928835,
0.233157223576062));
#5261=CARTESIAN_POINT('Ctrl Pts',(0.955173119738174,-0.099930567888331,
0.223801617934945));
#5262=CARTESIAN_POINT('Ctrl Pts',(0.960411259488514,-0.142345102874864,
0.199966927975188));
#5263=CARTESIAN_POINT('Ctrl Pts',(0.963103647174702,-0.15976606450048,0.1868781821531));
#5264=CARTESIAN_POINT('Ctrl Pts',(0.968453058988463,-0.190326085855194,
0.15681442133453));
#5265=CARTESIAN_POINT('Ctrl Pts',(0.971100730005489,-0.203463743702801,
0.139836317888042));
#5266=CARTESIAN_POINT('Ctrl Pts',(0.975530745318961,-0.224161999508995,
0.104422493053067));
#5267=CARTESIAN_POINT('Ctrl Pts',(0.977553872336861,-0.232861760990032,
0.0842175114474172));
#5268=CARTESIAN_POINT('Ctrl Pts',(0.980270995488453,-0.244251601209411,
0.0421062857595697));
#5269=CARTESIAN_POINT('Ctrl Pts',(0.980948,-0.246942143572133,0.0201990724523194));
#5270=CARTESIAN_POINT('Ctrl Pts',(0.980948,-0.246942143572133,-0.0201990724523194));
#5271=CARTESIAN_POINT('Ctrl Pts',(0.980270995488453,-0.244251601209411,
-0.0421062857595697));
#5272=CARTESIAN_POINT('Ctrl Pts',(0.977553872336861,-0.232861760990032,
-0.0842175114474172));
#5273=CARTESIAN_POINT('Ctrl Pts',(0.975530745318961,-0.224161999508995,
-0.104422493053067));
#5274=CARTESIAN_POINT('Ctrl Pts',(0.971100730005489,-0.203463743702801,
-0.139836317888042));
#5275=CARTESIAN_POINT('Ctrl Pts',(0.968453058988463,-0.190326085855194,
-0.15681442133453));
#5276=CARTESIAN_POINT('Ctrl Pts',(0.963103647174702,-0.15976606450048,-0.1868781821531));
#5277=CARTESIAN_POINT('Ctrl Pts',(0.960411259488514,-0.142345102874864,
-0.199966927975188));
#5278=CARTESIAN_POINT('Ctrl Pts',(0.955173119738174,-0.099930567888331,
-0.223801617934945));
#5279=CARTESIAN_POINT('Ctrl Pts',(0.952850216871763,-0.0740444353928835,
-0.233157223576062));
#5280=CARTESIAN_POINT('Ctrl Pts',(0.951592097314,-0.0476299999999999,-0.238183666596899));
#5281=CARTESIAN_POINT('Origin',(0.,-0.04763,0.));
#5282=CARTESIAN_POINT('Origin',(0.,-0.04763,0.));
#5283=CARTESIAN_POINT('Origin',(1.,-0.04763,0.));
#5284=CARTESIAN_POINT('Origin',(1.,0.,0.));
#5285=CARTESIAN_POINT('Origin',(1.,-0.04763,0.));
#5286=CARTESIAN_POINT('Origin',(0.,-0.28578,0.));
#5287=CARTESIAN_POINT('Origin',(0.,-0.04763,0.));
#5288=CARTESIAN_POINT('',(0.,0.,0.));
#5289=CARTESIAN_POINT('Origin',(1.013815,0.445,0.));
#5290=CARTESIAN_POINT('',(-1.013815,0.445,-1.24156529467757E-16));
#5291=CARTESIAN_POINT('Origin',(0.,0.445,0.));
#5292=CARTESIAN_POINT('',(-0.991185,0.445,-1.21385153761287E-16));
#5293=CARTESIAN_POINT('Origin',(0.,0.445,0.));
#5294=CARTESIAN_POINT('Origin',(0.,0.4075,0.));
#5295=CARTESIAN_POINT('',(-1.013815,0.37,-1.24156529467757E-16));
#5296=CARTESIAN_POINT('Origin',(0.,0.37,0.));
#5297=CARTESIAN_POINT('',(-1.013815,0.4075,-1.24156529467757E-16));
#5298=CARTESIAN_POINT('Origin',(0.991185,0.37,0.));
#5299=CARTESIAN_POINT('',(-0.991185,0.37,-1.21385153761287E-16));
#5300=CARTESIAN_POINT('Origin',(0.,0.37,0.));
#5301=CARTESIAN_POINT('Origin',(0.,0.4075,0.));
#5302=CARTESIAN_POINT('',(-0.991185,0.4075,-1.21385153761287E-16));
#5303=CARTESIAN_POINT('Origin',(1.013815,-0.37,0.));
#5304=CARTESIAN_POINT('',(-1.013815,-0.37,-1.24156529467757E-16));
#5305=CARTESIAN_POINT('Origin',(0.,-0.37,0.));
#5306=CARTESIAN_POINT('',(-0.991185,-0.37,-1.21385153761287E-16));
#5307=CARTESIAN_POINT('Origin',(0.,-0.37,0.));
#5308=CARTESIAN_POINT('Origin',(0.,-0.4075,0.));
#5309=CARTESIAN_POINT('',(-1.013815,-0.445,-1.24156529467757E-16));
#5310=CARTESIAN_POINT('Origin',(0.,-0.445,0.));
#5311=CARTESIAN_POINT('',(-1.013815,-0.4075,-1.24156529467757E-16));
#5312=CARTESIAN_POINT('Origin',(0.991185,-0.445,0.));
#5313=CARTESIAN_POINT('',(-0.991185,-0.445,-1.21385153761287E-16));
#5314=CARTESIAN_POINT('Origin',(0.,-0.445,0.));
#5315=CARTESIAN_POINT('Origin',(0.,-0.4075,0.));
#5316=CARTESIAN_POINT('',(-0.991185,-0.4075,-1.21385153761287E-16));
#5317=CARTESIAN_POINT('',(0.,0.,0.));
#5318=CARTESIAN_POINT('',(0.,0.,0.));
#5319=CARTESIAN_POINT('',(0.,0.,0.));
#5320=CARTESIAN_POINT('',(0.,0.,0.));
#5321=CARTESIAN_POINT('',(0.,0.,0.));
#5322=CARTESIAN_POINT('',(0.,0.,0.));
#5323=CARTESIAN_POINT('',(0.,0.,0.));
#5324=CARTESIAN_POINT('',(0.,0.,0.));
#5325=CARTESIAN_POINT('',(0.,-0.6,4.));
#5326=CARTESIAN_POINT('',(0.,0.6,4.));
#5327=CARTESIAN_POINT('',(0.,0.,0.));
#5328=CARTESIAN_POINT('',(0.,0.,0.));
#5329=CARTESIAN_POINT('',(0.,0.,0.));
#5330=UNCERTAINTY_MEASURE_WITH_UNIT(LENGTH_MEASURE(0.001),#5386,
'DISTANCE_ACCURACY_VALUE',
'Maximum model space distance between geometric entities at asserted c
onnectivities');
#5331=UNCERTAINTY_MEASURE_WITH_UNIT(LENGTH_MEASURE(0.001),#5386,
'DISTANCE_ACCURACY_VALUE',
'Maximum model space distance between geometric entities at asserted c
onnectivities');
#5332=UNCERTAINTY_MEASURE_WITH_UNIT(LENGTH_MEASURE(0.001),#5386,
'DISTANCE_ACCURACY_VALUE',
'Maximum model space distance between geometric entities at asserted c
onnectivities');
#5333=UNCERTAINTY_MEASURE_WITH_UNIT(LENGTH_MEASURE(0.001),#5386,
'DISTANCE_ACCURACY_VALUE',
'Maximum model space distance between geometric entities at asserted c
onnectivities');
#5334=UNCERTAINTY_MEASURE_WITH_UNIT(LENGTH_MEASURE(0.001),#5386,
'DISTANCE_ACCURACY_VALUE',
'Maximum model space distance between geometric entities at asserted c
onnectivities');
#5335=UNCERTAINTY_MEASURE_WITH_UNIT(LENGTH_MEASURE(0.001),#5386,
'DISTANCE_ACCURACY_VALUE',
'Maximum model space distance between geometric entities at asserted c
onnectivities');
#5336=UNCERTAINTY_MEASURE_WITH_UNIT(LENGTH_MEASURE(0.001),#5386,
'DISTANCE_ACCURACY_VALUE',
'Maximum model space distance between geometric entities at asserted c
onnectivities');
#5337=UNCERTAINTY_MEASURE_WITH_UNIT(LENGTH_MEASURE(0.001),#5386,
'DISTANCE_ACCURACY_VALUE',
'Maximum model space distance between geometric entities at asserted c
onnectivities');
#5338=UNCERTAINTY_MEASURE_WITH_UNIT(LENGTH_MEASURE(0.001),#5386,
'DISTANCE_ACCURACY_VALUE',
'Maximum model space distance between geometric entities at asserted c
onnectivities');
#5339=UNCERTAINTY_MEASURE_WITH_UNIT(LENGTH_MEASURE(0.001),#5386,
'DISTANCE_ACCURACY_VALUE',
'Maximum model space distance between geometric entities at asserted c
onnectivities');
#5340=UNCERTAINTY_MEASURE_WITH_UNIT(LENGTH_MEASURE(0.001),#5386,
'DISTANCE_ACCURACY_VALUE',
'Maximum model space distance between geometric entities at asserted c
onnectivities');
#5341=UNCERTAINTY_MEASURE_WITH_UNIT(LENGTH_MEASURE(0.001),#5386,
'DISTANCE_ACCURACY_VALUE',
'Maximum model space distance between geometric entities at asserted c
onnectivities');
#5342=UNCERTAINTY_MEASURE_WITH_UNIT(LENGTH_MEASURE(0.001),#5386,
'DISTANCE_ACCURACY_VALUE',
'Maximum model space distance between geometric entities at asserted c
onnectivities');
#5343=UNCERTAINTY_MEASURE_WITH_UNIT(LENGTH_MEASURE(0.001),#5386,
'DISTANCE_ACCURACY_VALUE',
'Maximum model space distance between geometric entities at asserted c
onnectivities');
#5344=UNCERTAINTY_MEASURE_WITH_UNIT(LENGTH_MEASURE(0.001),#5386,
'DISTANCE_ACCURACY_VALUE',
'Maximum model space distance between geometric entities at asserted c
onnectivities');
#5345=UNCERTAINTY_MEASURE_WITH_UNIT(LENGTH_MEASURE(0.001),#5386,
'DISTANCE_ACCURACY_VALUE',
'Maximum model space distance between geometric entities at asserted c
onnectivities');
#5346=UNCERTAINTY_MEASURE_WITH_UNIT(LENGTH_MEASURE(0.001),#5386,
'DISTANCE_ACCURACY_VALUE',
'Maximum model space distance between geometric entities at asserted c
onnectivities');
#5347=UNCERTAINTY_MEASURE_WITH_UNIT(LENGTH_MEASURE(0.001),#5386,
'DISTANCE_ACCURACY_VALUE',
'Maximum model space distance between geometric entities at asserted c
onnectivities');
#5348=UNCERTAINTY_MEASURE_WITH_UNIT(LENGTH_MEASURE(0.001),#5386,
'DISTANCE_ACCURACY_VALUE',
'Maximum model space distance between geometric entities at asserted c
onnectivities');
#5349=UNCERTAINTY_MEASURE_WITH_UNIT(LENGTH_MEASURE(0.001),#5386,
'DISTANCE_ACCURACY_VALUE',
'Maximum model space distance between geometric entities at asserted c
onnectivities');
#5350=UNCERTAINTY_MEASURE_WITH_UNIT(LENGTH_MEASURE(0.001),#5386,
'DISTANCE_ACCURACY_VALUE',
'Maximum model space distance between geometric entities at asserted c
onnectivities');
#5351=UNCERTAINTY_MEASURE_WITH_UNIT(LENGTH_MEASURE(0.001),#5386,
'DISTANCE_ACCURACY_VALUE',
'Maximum model space distance between geometric entities at asserted c
onnectivities');
#5352=UNCERTAINTY_MEASURE_WITH_UNIT(LENGTH_MEASURE(0.001),#5386,
'DISTANCE_ACCURACY_VALUE',
'Maximum model space distance between geometric entities at asserted c
onnectivities');
#5353=UNCERTAINTY_MEASURE_WITH_UNIT(LENGTH_MEASURE(0.001),#5386,
'DISTANCE_ACCURACY_VALUE',
'Maximum model space distance between geometric entities at asserted c
onnectivities');
#5354=UNCERTAINTY_MEASURE_WITH_UNIT(LENGTH_MEASURE(0.001),#5386,
'DISTANCE_ACCURACY_VALUE',
'Maximum model space distance between geometric entities at asserted c
onnectivities');
#5355=UNCERTAINTY_MEASURE_WITH_UNIT(LENGTH_MEASURE(0.001),#5386,
'DISTANCE_ACCURACY_VALUE',
'Maximum model space distance between geometric entities at asserted c
onnectivities');
#5356=UNCERTAINTY_MEASURE_WITH_UNIT(LENGTH_MEASURE(0.001),#5386,
'DISTANCE_ACCURACY_VALUE',
'Maximum model space distance between geometric entities at asserted c
onnectivities');
#5357=UNCERTAINTY_MEASURE_WITH_UNIT(LENGTH_MEASURE(0.001),#5386,
'DISTANCE_ACCURACY_VALUE',
'Maximum model space distance between geometric entities at asserted c
onnectivities');
#5358=(
GEOMETRIC_REPRESENTATION_CONTEXT(3)
GLOBAL_UNCERTAINTY_ASSIGNED_CONTEXT((#5330))
GLOBAL_UNIT_ASSIGNED_CONTEXT((#5386,#5388,#5389))
REPRESENTATION_CONTEXT('','3D')
);
#5359=(
GEOMETRIC_REPRESENTATION_CONTEXT(3)
GLOBAL_UNCERTAINTY_ASSIGNED_CONTEXT((#5331))
GLOBAL_UNIT_ASSIGNED_CONTEXT((#5386,#5388,#5389))
REPRESENTATION_CONTEXT('','3D')
);
#5360=(
GEOMETRIC_REPRESENTATION_CONTEXT(3)
GLOBAL_UNCERTAINTY_ASSIGNED_CONTEXT((#5332))
GLOBAL_UNIT_ASSIGNED_CONTEXT((#5386,#5388,#5389))
REPRESENTATION_CONTEXT('','3D')
);
#5361=(
GEOMETRIC_REPRESENTATION_CONTEXT(3)
GLOBAL_UNCERTAINTY_ASSIGNED_CONTEXT((#5333))
GLOBAL_UNIT_ASSIGNED_CONTEXT((#5386,#5388,#5389))
REPRESENTATION_CONTEXT('','3D')
);
#5362=(
GEOMETRIC_REPRESENTATION_CONTEXT(3)
GLOBAL_UNCERTAINTY_ASSIGNED_CONTEXT((#5334))
GLOBAL_UNIT_ASSIGNED_CONTEXT((#5386,#5388,#5389))
REPRESENTATION_CONTEXT('','3D')
);
#5363=(
GEOMETRIC_REPRESENTATION_CONTEXT(3)
GLOBAL_UNCERTAINTY_ASSIGNED_CONTEXT((#5335))
GLOBAL_UNIT_ASSIGNED_CONTEXT((#5386,#5388,#5389))
REPRESENTATION_CONTEXT('','3D')
);
#5364=(
GEOMETRIC_REPRESENTATION_CONTEXT(3)
GLOBAL_UNCERTAINTY_ASSIGNED_CONTEXT((#5336))
GLOBAL_UNIT_ASSIGNED_CONTEXT((#5386,#5388,#5389))
REPRESENTATION_CONTEXT('','3D')
);
#5365=(
GEOMETRIC_REPRESENTATION_CONTEXT(3)
GLOBAL_UNCERTAINTY_ASSIGNED_CONTEXT((#5337))
GLOBAL_UNIT_ASSIGNED_CONTEXT((#5386,#5388,#5389))
REPRESENTATION_CONTEXT('','3D')
);
#5366=(
GEOMETRIC_REPRESENTATION_CONTEXT(3)
GLOBAL_UNCERTAINTY_ASSIGNED_CONTEXT((#5338))
GLOBAL_UNIT_ASSIGNED_CONTEXT((#5386,#5388,#5389))
REPRESENTATION_CONTEXT('','3D')
);
#5367=(
GEOMETRIC_REPRESENTATION_CONTEXT(3)
GLOBAL_UNCERTAINTY_ASSIGNED_CONTEXT((#5339))
GLOBAL_UNIT_ASSIGNED_CONTEXT((#5386,#5388,#5389))
REPRESENTATION_CONTEXT('','3D')
);
#5368=(
GEOMETRIC_REPRESENTATION_CONTEXT(3)
GLOBAL_UNCERTAINTY_ASSIGNED_CONTEXT((#5340))
GLOBAL_UNIT_ASSIGNED_CONTEXT((#5386,#5388,#5389))
REPRESENTATION_CONTEXT('','3D')
);
#5369=(
GEOMETRIC_REPRESENTATION_CONTEXT(3)
GLOBAL_UNCERTAINTY_ASSIGNED_CONTEXT((#5341))
GLOBAL_UNIT_ASSIGNED_CONTEXT((#5386,#5388,#5389))
REPRESENTATION_CONTEXT('','3D')
);
#5370=(
GEOMETRIC_REPRESENTATION_CONTEXT(3)
GLOBAL_UNCERTAINTY_ASSIGNED_CONTEXT((#5342))
GLOBAL_UNIT_ASSIGNED_CONTEXT((#5386,#5388,#5389))
REPRESENTATION_CONTEXT('','3D')
);
#5371=(
GEOMETRIC_REPRESENTATION_CONTEXT(3)
GLOBAL_UNCERTAINTY_ASSIGNED_CONTEXT((#5343))
GLOBAL_UNIT_ASSIGNED_CONTEXT((#5386,#5388,#5389))
REPRESENTATION_CONTEXT('','3D')
);
#5372=(
GEOMETRIC_REPRESENTATION_CONTEXT(3)
GLOBAL_UNCERTAINTY_ASSIGNED_CONTEXT((#5344))
GLOBAL_UNIT_ASSIGNED_CONTEXT((#5386,#5388,#5389))
REPRESENTATION_CONTEXT('','3D')
);
#5373=(
GEOMETRIC_REPRESENTATION_CONTEXT(3)
GLOBAL_UNCERTAINTY_ASSIGNED_CONTEXT((#5345))
GLOBAL_UNIT_ASSIGNED_CONTEXT((#5386,#5388,#5389))
REPRESENTATION_CONTEXT('','3D')
);
#5374=(
GEOMETRIC_REPRESENTATION_CONTEXT(3)
GLOBAL_UNCERTAINTY_ASSIGNED_CONTEXT((#5346))
GLOBAL_UNIT_ASSIGNED_CONTEXT((#5386,#5388,#5389))
REPRESENTATION_CONTEXT('','3D')
);
#5375=(
GEOMETRIC_REPRESENTATION_CONTEXT(3)
GLOBAL_UNCERTAINTY_ASSIGNED_CONTEXT((#5347))
GLOBAL_UNIT_ASSIGNED_CONTEXT((#5386,#5388,#5389))
REPRESENTATION_CONTEXT('','3D')
);
#5376=(
GEOMETRIC_REPRESENTATION_CONTEXT(3)
GLOBAL_UNCERTAINTY_ASSIGNED_CONTEXT((#5348))
GLOBAL_UNIT_ASSIGNED_CONTEXT((#5386,#5388,#5389))
REPRESENTATION_CONTEXT('','3D')
);
#5377=(
GEOMETRIC_REPRESENTATION_CONTEXT(3)
GLOBAL_UNCERTAINTY_ASSIGNED_CONTEXT((#5349))
GLOBAL_UNIT_ASSIGNED_CONTEXT((#5386,#5388,#5389))
REPRESENTATION_CONTEXT('','3D')
);
#5378=(
GEOMETRIC_REPRESENTATION_CONTEXT(3)
GLOBAL_UNCERTAINTY_ASSIGNED_CONTEXT((#5350))
GLOBAL_UNIT_ASSIGNED_CONTEXT((#5386,#5388,#5389))
REPRESENTATION_CONTEXT('','3D')
);
#5379=(
GEOMETRIC_REPRESENTATION_CONTEXT(3)
GLOBAL_UNCERTAINTY_ASSIGNED_CONTEXT((#5351))
GLOBAL_UNIT_ASSIGNED_CONTEXT((#5386,#5388,#5389))
REPRESENTATION_CONTEXT('','3D')
);
#5380=(
GEOMETRIC_REPRESENTATION_CONTEXT(3)
GLOBAL_UNCERTAINTY_ASSIGNED_CONTEXT((#5352))
GLOBAL_UNIT_ASSIGNED_CONTEXT((#5386,#5388,#5389))
REPRESENTATION_CONTEXT('','3D')
);
#5381=(
GEOMETRIC_REPRESENTATION_CONTEXT(3)
GLOBAL_UNCERTAINTY_ASSIGNED_CONTEXT((#5353))
GLOBAL_UNIT_ASSIGNED_CONTEXT((#5386,#5388,#5389))
REPRESENTATION_CONTEXT('','3D')
);
#5382=(
GEOMETRIC_REPRESENTATION_CONTEXT(3)
GLOBAL_UNCERTAINTY_ASSIGNED_CONTEXT((#5354))
GLOBAL_UNIT_ASSIGNED_CONTEXT((#5386,#5388,#5389))
REPRESENTATION_CONTEXT('','3D')
);
#5383=(
GEOMETRIC_REPRESENTATION_CONTEXT(3)
GLOBAL_UNCERTAINTY_ASSIGNED_CONTEXT((#5355))
GLOBAL_UNIT_ASSIGNED_CONTEXT((#5386,#5388,#5389))
REPRESENTATION_CONTEXT('','3D')
);
#5384=(
GEOMETRIC_REPRESENTATION_CONTEXT(3)
GLOBAL_UNCERTAINTY_ASSIGNED_CONTEXT((#5356))
GLOBAL_UNIT_ASSIGNED_CONTEXT((#5386,#5388,#5389))
REPRESENTATION_CONTEXT('','3D')
);
#5385=(
GEOMETRIC_REPRESENTATION_CONTEXT(3)
GLOBAL_UNCERTAINTY_ASSIGNED_CONTEXT((#5357))
GLOBAL_UNIT_ASSIGNED_CONTEXT((#5386,#5388,#5389))
REPRESENTATION_CONTEXT('','3D')
);
#5386=(
LENGTH_UNIT()
NAMED_UNIT(*)
SI_UNIT(.CENTI.,.METRE.)
);
#5387=(
LENGTH_UNIT()
NAMED_UNIT(*)
SI_UNIT($,.METRE.)
);
#5388=(
NAMED_UNIT(*)
PLANE_ANGLE_UNIT()
SI_UNIT($,.RADIAN.)
);
#5389=(
NAMED_UNIT(*)
SI_UNIT($,.STERADIAN.)
SOLID_ANGLE_UNIT()
);
#5390=SHAPE_DEFINITION_REPRESENTATION(#5417,#5471);
#5391=SHAPE_DEFINITION_REPRESENTATION(#5418,#5472);
#5392=SHAPE_DEFINITION_REPRESENTATION(#5419,#5473);
#5393=SHAPE_DEFINITION_REPRESENTATION(#5420,#5474);
#5394=SHAPE_DEFINITION_REPRESENTATION(#5421,#5475);
#5395=SHAPE_DEFINITION_REPRESENTATION(#5422,#5476);
#5396=SHAPE_DEFINITION_REPRESENTATION(#5423,#5477);
#5397=SHAPE_DEFINITION_REPRESENTATION(#5429,#5478);
#5398=SHAPE_DEFINITION_REPRESENTATION(#5430,#5479);
#5399=SHAPE_DEFINITION_REPRESENTATION(#5431,#5480);
#5400=SHAPE_DEFINITION_REPRESENTATION(#5432,#5481);
#5401=SHAPE_DEFINITION_REPRESENTATION(#5433,#5482);
#5402=SHAPE_DEFINITION_REPRESENTATION(#5434,#5483);
#5403=SHAPE_DEFINITION_REPRESENTATION(#5435,#5484);
#5404=SHAPE_DEFINITION_REPRESENTATION(#5436,#5485);
#5405=SHAPE_DEFINITION_REPRESENTATION(#5437,#5486);
#5406=SHAPE_DEFINITION_REPRESENTATION(#5438,#5487);
#5407=SHAPE_DEFINITION_REPRESENTATION(#5448,#5488);
#5408=SHAPE_DEFINITION_REPRESENTATION(#5449,#5489);
#5409=SHAPE_DEFINITION_REPRESENTATION(#5450,#5490);
#5410=SHAPE_DEFINITION_REPRESENTATION(#5451,#5491);
#5411=SHAPE_DEFINITION_REPRESENTATION(#5452,#5492);
#5412=SHAPE_DEFINITION_REPRESENTATION(#5453,#5493);
#5413=SHAPE_DEFINITION_REPRESENTATION(#5454,#5494);
#5414=SHAPE_DEFINITION_REPRESENTATION(#5455,#5495);
#5415=SHAPE_DEFINITION_REPRESENTATION(#5456,#5496);
#5416=SHAPE_DEFINITION_REPRESENTATION(#5457,#5497);
#5417=PRODUCT_DEFINITION_SHAPE('',$,#5499);
#5418=PRODUCT_DEFINITION_SHAPE('',$,#5500);
#5419=PRODUCT_DEFINITION_SHAPE('',$,#5501);
#5420=PRODUCT_DEFINITION_SHAPE('',$,#5502);
#5421=PRODUCT_DEFINITION_SHAPE('',$,#5503);
#5422=PRODUCT_DEFINITION_SHAPE('',$,#5504);
#5423=PRODUCT_DEFINITION_SHAPE('',$,#5505);
#5424=PRODUCT_DEFINITION_SHAPE($,$,#130);
#5425=PRODUCT_DEFINITION_SHAPE($,$,#131);
#5426=PRODUCT_DEFINITION_SHAPE($,$,#132);
#5427=PRODUCT_DEFINITION_SHAPE($,$,#133);
#5428=PRODUCT_DEFINITION_SHAPE($,$,#134);
#5429=PRODUCT_DEFINITION_SHAPE('',$,#5506);
#5430=PRODUCT_DEFINITION_SHAPE('',$,#5507);
#5431=PRODUCT_DEFINITION_SHAPE('',$,#5508);
#5432=PRODUCT_DEFINITION_SHAPE('',$,#5509);
#5433=PRODUCT_DEFINITION_SHAPE('',$,#5510);
#5434=PRODUCT_DEFINITION_SHAPE('',$,#5511);
#5435=PRODUCT_DEFINITION_SHAPE('',$,#5512);
#5436=PRODUCT_DEFINITION_SHAPE('',$,#5513);
#5437=PRODUCT_DEFINITION_SHAPE('',$,#5514);
#5438=PRODUCT_DEFINITION_SHAPE('',$,#5515);
#5439=PRODUCT_DEFINITION_SHAPE($,$,#135);
#5440=PRODUCT_DEFINITION_SHAPE($,$,#136);
#5441=PRODUCT_DEFINITION_SHAPE($,$,#137);
#5442=PRODUCT_DEFINITION_SHAPE($,$,#138);
#5443=PRODUCT_DEFINITION_SHAPE($,$,#139);
#5444=PRODUCT_DEFINITION_SHAPE($,$,#140);
#5445=PRODUCT_DEFINITION_SHAPE($,$,#141);
#5446=PRODUCT_DEFINITION_SHAPE($,$,#142);
#5447=PRODUCT_DEFINITION_SHAPE($,$,#143);
#5448=PRODUCT_DEFINITION_SHAPE('',$,#5516);
#5449=PRODUCT_DEFINITION_SHAPE('',$,#5517);
#5450=PRODUCT_DEFINITION_SHAPE('',$,#5518);
#5451=PRODUCT_DEFINITION_SHAPE('',$,#5519);
#5452=PRODUCT_DEFINITION_SHAPE('',$,#5520);
#5453=PRODUCT_DEFINITION_SHAPE('',$,#5521);
#5454=PRODUCT_DEFINITION_SHAPE('',$,#5522);
#5455=PRODUCT_DEFINITION_SHAPE('',$,#5523);
#5456=PRODUCT_DEFINITION_SHAPE('',$,#5524);
#5457=PRODUCT_DEFINITION_SHAPE('',$,#5525);
#5458=PRODUCT_DEFINITION_SHAPE($,$,#144);
#5459=PRODUCT_DEFINITION_SHAPE($,$,#145);
#5460=PRODUCT_DEFINITION_SHAPE($,$,#146);
#5461=PRODUCT_DEFINITION_SHAPE($,$,#147);
#5462=PRODUCT_DEFINITION_SHAPE($,$,#148);
#5463=PRODUCT_DEFINITION_SHAPE($,$,#149);
#5464=PRODUCT_DEFINITION_SHAPE($,$,#150);
#5465=PRODUCT_DEFINITION_SHAPE($,$,#151);
#5466=PRODUCT_DEFINITION_SHAPE($,$,#152);
#5467=PRODUCT_DEFINITION_SHAPE($,$,#153);
#5468=PRODUCT_DEFINITION_SHAPE($,$,#154);
#5469=PRODUCT_DEFINITION_SHAPE($,$,#155);
#5470=PRODUCT_DEFINITION_SHAPE($,$,#156);
#5471=SHAPE_REPRESENTATION('',(#2923,#3301,#3302,#3303),#5358);
#5472=SHAPE_REPRESENTATION('',(#2924,#2995,#2996,#2997,#2998,#2999),#5359);
#5473=SHAPE_REPRESENTATION('',(#2925),#5360);
#5474=SHAPE_REPRESENTATION('',(#2947),#5361);
#5475=SHAPE_REPRESENTATION('',(#2961),#5362);
#5476=SHAPE_REPRESENTATION('',(#2970),#5363);
#5477=SHAPE_REPRESENTATION('',(#2979),#5364);
#5478=SHAPE_REPRESENTATION('',(#3000,#3117,#3118,#3119,#3120,#3121,#3122,
#3123,#3124,#3125),#5365);
#5479=SHAPE_REPRESENTATION('',(#3001),#5366);
#5480=SHAPE_REPRESENTATION('',(#3025),#5367);
#5481=SHAPE_REPRESENTATION('',(#3034),#5368);
#5482=SHAPE_REPRESENTATION('',(#3043),#5369);
#5483=SHAPE_REPRESENTATION('',(#3052),#5370);
#5484=SHAPE_REPRESENTATION('',(#3066),#5371);
#5485=SHAPE_REPRESENTATION('',(#3075),#5372);
#5486=SHAPE_REPRESENTATION('',(#3084),#5373);
#5487=SHAPE_REPRESENTATION('',(#3093),#5374);
#5488=SHAPE_REPRESENTATION('',(#3126,#3296,#3297,#3298,#3299,#3300),#5375);
#5489=SHAPE_REPRESENTATION('',(#3127),#5376);
#5490=SHAPE_REPRESENTATION('',(#3144),#5377);
#5491=SHAPE_REPRESENTATION('',(#3153),#5378);
#5492=SHAPE_REPRESENTATION('',(#3162,#3291,#3292,#3293,#3294,#3295),#5379);
#5493=SHAPE_REPRESENTATION('',(#3163),#5380);
#5494=SHAPE_REPRESENTATION('',(#3183),#5381);
#5495=SHAPE_REPRESENTATION('',(#3203),#5382);
#5496=SHAPE_REPRESENTATION('',(#3220),#5383);
#5497=SHAPE_REPRESENTATION('',(#3274),#5384);
#5498=PRODUCT_DEFINITION_CONTEXT('part definition',#5581,'design');
#5499=PRODUCT_DEFINITION('PAT-019','PAT-019',#5526,#5498);
#5500=PRODUCT_DEFINITION('Mounting plate and kingpin',
'Mounting plate and kingpin',#5527,#5498);
#5501=PRODUCT_DEFINITION('Mounting plate','Mounting plate',#5528,#5498);
#5502=PRODUCT_DEFINITION('Kingpin','Kingpin',#5529,#5498);
#5503=PRODUCT_DEFINITION('Upper thrust race','Upper thrust race',#5530,
#5498);
#5504=PRODUCT_DEFINITION('Flat Washer - M8','Flat Washer - M8',#5531,#5498);
#5505=PRODUCT_DEFINITION('Hex Nut - M8','Hex Nut - M8',#5532,#5498);
#5506=PRODUCT_DEFINITION('Swivel fork','Swivel fork',#5533,#5498);
#5507=PRODUCT_DEFINITION('Fork','Fork',#5534,#5498);
#5508=PRODUCT_DEFINITION('Swivel bushing','Swivel bushing',#5535,#5498);
#5509=PRODUCT_DEFINITION('Lower thrust race','Lower thrust race',#5536,
#5498);
#5510=PRODUCT_DEFINITION('Dust shield','Dust shield',#5537,#5498);
#5511=PRODUCT_DEFINITION('Wheel axle','Wheel axle',#5538,#5498);
#5512=PRODUCT_DEFINITION('Inner race spacer','Inner race spacer',#5539,
#5498);
#5513=PRODUCT_DEFINITION('Inner race spacer (1)','Inner race spacer (1)',
#5540,#5498);
#5514=PRODUCT_DEFINITION('Axle keeper','Axle keeper',#5541,#5498);
#5515=PRODUCT_DEFINITION('M4x10 Cap Screw','M4x10 Cap Screw',#5542,#5498);
#5516=PRODUCT_DEFINITION('Wheel and bearings','Wheel and bearings',#5543,
#5498);
#5517=PRODUCT_DEFINITION('Wheel','Wheel',#5544,#5498);
#5518=PRODUCT_DEFINITION('Wheel bearing retainer',
'Wheel bearing retainer',#5545,#5498);
#5519=PRODUCT_DEFINITION('Wheel bearing retainer (1)',
'Wheel bearing retainer (1)',#5546,#5498);
#5520=PRODUCT_DEFINITION('Sealed Ball Bearing - 10 x 30 x 9 mm',
'Sealed Ball Bearing - 10 x 30 x 9 mm',#5547,#5498);
#5521=PRODUCT_DEFINITION('Inner ring','Inner ring',#5548,#5498);
#5522=PRODUCT_DEFINITION('Outer ring','Outer ring',#5549,#5498);
#5523=PRODUCT_DEFINITION('Balls','Balls',#5550,#5498);
#5524=PRODUCT_DEFINITION('Cage','Cage',#5551,#5498);
#5525=PRODUCT_DEFINITION('Seals 2RS','Seals 2RS',#5552,#5498);
#5526=PRODUCT_DEFINITION_FORMATION('',$,#5583);
#5527=PRODUCT_DEFINITION_FORMATION('',$,#5584);
#5528=PRODUCT_DEFINITION_FORMATION('',$,#5585);
#5529=PRODUCT_DEFINITION_FORMATION('',$,#5586);
#5530=PRODUCT_DEFINITION_FORMATION('',$,#5587);
#5531=PRODUCT_DEFINITION_FORMATION('',$,#5588);
#5532=PRODUCT_DEFINITION_FORMATION('',$,#5589);
#5533=PRODUCT_DEFINITION_FORMATION('',$,#5590);
#5534=PRODUCT_DEFINITION_FORMATION('',$,#5591);
#5535=PRODUCT_DEFINITION_FORMATION('',$,#5592);
#5536=PRODUCT_DEFINITION_FORMATION('',$,#5593);
#5537=PRODUCT_DEFINITION_FORMATION('',$,#5594);
#5538=PRODUCT_DEFINITION_FORMATION('',$,#5595);
#5539=PRODUCT_DEFINITION_FORMATION('',$,#5596);
#5540=PRODUCT_DEFINITION_FORMATION('',$,#5597);
#5541=PRODUCT_DEFINITION_FORMATION('',$,#5598);
#5542=PRODUCT_DEFINITION_FORMATION('',$,#5599);
#5543=PRODUCT_DEFINITION_FORMATION('',$,#5600);
#5544=PRODUCT_DEFINITION_FORMATION('',$,#5601);
#5545=PRODUCT_DEFINITION_FORMATION('',$,#5602);
#5546=PRODUCT_DEFINITION_FORMATION('',$,#5603);
#5547=PRODUCT_DEFINITION_FORMATION('',$,#5604);
#5548=PRODUCT_DEFINITION_FORMATION('',$,#5605);
#5549=PRODUCT_DEFINITION_FORMATION('',$,#5606);
#5550=PRODUCT_DEFINITION_FORMATION('',$,#5607);
#5551=PRODUCT_DEFINITION_FORMATION('',$,#5608);
#5552=PRODUCT_DEFINITION_FORMATION('',$,#5609);
#5553=PRODUCT_RELATED_PRODUCT_CATEGORY('PAT-019','PAT-019',(#5583));
#5554=PRODUCT_RELATED_PRODUCT_CATEGORY('Mounting plate and kingpin',
'Mounting plate and kingpin',(#5584));
#5555=PRODUCT_RELATED_PRODUCT_CATEGORY('Mounting plate',
'Mounting plate',(#5585));
#5556=PRODUCT_RELATED_PRODUCT_CATEGORY('Kingpin','Kingpin',(#5586));
#5557=PRODUCT_RELATED_PRODUCT_CATEGORY('Upper thrust race',
'Upper thrust race',(#5587));
#5558=PRODUCT_RELATED_PRODUCT_CATEGORY('Flat Washer - M8',
'Flat Washer - M8',(#5588));
#5559=PRODUCT_RELATED_PRODUCT_CATEGORY('Hex Nut - M8','Hex Nut - M8',(#5589));
#5560=PRODUCT_RELATED_PRODUCT_CATEGORY('Swivel fork','Swivel fork',(#5590));
#5561=PRODUCT_RELATED_PRODUCT_CATEGORY('Fork','Fork',(#5591));
#5562=PRODUCT_RELATED_PRODUCT_CATEGORY('Swivel bushing',
'Swivel bushing',(#5592));
#5563=PRODUCT_RELATED_PRODUCT_CATEGORY('Lower thrust race',
'Lower thrust race',(#5593));
#5564=PRODUCT_RELATED_PRODUCT_CATEGORY('Dust shield','Dust shield',(#5594));
#5565=PRODUCT_RELATED_PRODUCT_CATEGORY('Wheel axle','Wheel axle',(#5595));
#5566=PRODUCT_RELATED_PRODUCT_CATEGORY('Inner race spacer',
'Inner race spacer',(#5596));
#5567=PRODUCT_RELATED_PRODUCT_CATEGORY('Inner race spacer (1)',
'Inner race spacer (1)',(#5597));
#5568=PRODUCT_RELATED_PRODUCT_CATEGORY('Axle keeper','Axle keeper',(#5598));
#5569=PRODUCT_RELATED_PRODUCT_CATEGORY('M4x10 Cap Screw',
'M4x10 Cap Screw',(#5599));
#5570=PRODUCT_RELATED_PRODUCT_CATEGORY('Wheel and bearings',
'Wheel and bearings',(#5600));
#5571=PRODUCT_RELATED_PRODUCT_CATEGORY('Wheel','Wheel',(#5601));
#5572=PRODUCT_RELATED_PRODUCT_CATEGORY('Wheel bearing retainer',
'Wheel bearing retainer',(#5602));
#5573=PRODUCT_RELATED_PRODUCT_CATEGORY('Wheel bearing retainer (1)',
'Wheel bearing retainer (1)',(#5603));
#5574=PRODUCT_RELATED_PRODUCT_CATEGORY(
'Sealed Ball Bearing - 10 x 30 x 9 mm',
'Sealed Ball Bearing - 10 x 30 x 9 mm',(#5604));
#5575=PRODUCT_RELATED_PRODUCT_CATEGORY('Inner ring','Inner ring',(#5605));
#5576=PRODUCT_RELATED_PRODUCT_CATEGORY('Outer ring','Outer ring',(#5606));
#5577=PRODUCT_RELATED_PRODUCT_CATEGORY('Balls','Balls',(#5607));
#5578=PRODUCT_RELATED_PRODUCT_CATEGORY('Cage','Cage',(#5608));
#5579=PRODUCT_RELATED_PRODUCT_CATEGORY('Seals 2RS','Seals 2RS',(#5609));
#5580=APPLICATION_PROTOCOL_DEFINITION('international standard',
'automotive_design',2009,#5581);
#5581=APPLICATION_CONTEXT(
'Core Data for Automotive Mechanical Design Process');
#5582=PRODUCT_CONTEXT('part definition',#5581,'mechanical');
#5583=PRODUCT('PAT-019','PAT-019',
'PAT-019',(#5582));
#5584=PRODUCT('Mounting plate and kingpin','Mounting plate and kingpin',
'Mounting plate and kingpin',(#5582));
#5585=PRODUCT('Mounting plate','Mounting plate','Mounting plate',(#5582));
#5586=PRODUCT('Kingpin','Kingpin','Kingpin',(#5582));
#5587=PRODUCT('Upper thrust race','Upper thrust race',
'Upper thrust race',(#5582));
#5588=PRODUCT('Flat Washer - M8','Flat Washer - M8','Flat Washer - M8',
(#5582));
#5589=PRODUCT('Hex Nut - M8','Hex Nut - M8','Hex Nut - M8',(#5582));
#5590=PRODUCT('Swivel fork','Swivel fork','Swivel fork',(#5582));
#5591=PRODUCT('Fork','Fork','Fork',(#5582));
#5592=PRODUCT('Swivel bushing','Swivel bushing','Swivel bushing',(#5582));
#5593=PRODUCT('Lower thrust race','Lower thrust race',
'Lower thrust race',(#5582));
#5594=PRODUCT('Dust shield','Dust shield','Dust shield',(#5582));
#5595=PRODUCT('Wheel axle','Wheel axle','Wheel axle',(#5582));
#5596=PRODUCT('Inner race spacer','Inner race spacer',
'Inner race spacer',(#5582));
#5597=PRODUCT('Inner race spacer (1)','Inner race spacer (1)',
'Inner race spacer (1)',(#5582));
#5598=PRODUCT('Axle keeper','Axle keeper','Axle keeper',(#5582));
#5599=PRODUCT('M4x10 Cap Screw','M4x10 Cap Screw','M4x10 Cap Screw',(#5582));
#5600=PRODUCT('Wheel and bearings','Wheel and bearings',
'Wheel and bearings',(#5582));
#5601=PRODUCT('Wheel','Wheel','Wheel',(#5582));
#5602=PRODUCT('Wheel bearing retainer','Wheel bearing retainer',
'Wheel bearing retainer',(#5582));
#5603=PRODUCT('Wheel bearing retainer (1)','Wheel bearing retainer (1)',
'Wheel bearing retainer (1)',(#5582));
#5604=PRODUCT('Sealed Ball Bearing - 10 x 30 x 9 mm',
'Sealed Ball Bearing - 10 x 30 x 9 mm',
'Sealed Ball Bearing - 10 x 30 x 9 mm',(#5582));
#5605=PRODUCT('Inner ring','Inner ring','Inner ring',(#5582));
#5606=PRODUCT('Outer ring','Outer ring','Outer ring',(#5582));
#5607=PRODUCT('Balls','Balls','Balls',(#5582));
#5608=PRODUCT('Cage','Cage','Cage',(#5582));
#5609=PRODUCT('Seals 2RS','Seals 2RS','Seals 2RS',(#5582));
#5610=PRESENTATION_STYLE_ASSIGNMENT((#5615));
#5611=PRESENTATION_STYLE_ASSIGNMENT((#5616));
#5612=PRESENTATION_STYLE_ASSIGNMENT((#5617));
#5613=PRESENTATION_STYLE_ASSIGNMENT((#5618));
#5614=PRESENTATION_STYLE_ASSIGNMENT((#5619));
#5615=SURFACE_STYLE_USAGE(.BOTH.,#5620);
#5616=SURFACE_STYLE_USAGE(.BOTH.,#5621);
#5617=SURFACE_STYLE_USAGE(.BOTH.,#5622);
#5618=SURFACE_STYLE_USAGE(.BOTH.,#5623);
#5619=SURFACE_STYLE_USAGE(.BOTH.,#5624);
#5620=SURFACE_SIDE_STYLE('',(#5625));
#5621=SURFACE_SIDE_STYLE('',(#5626));
#5622=SURFACE_SIDE_STYLE('',(#5627));
#5623=SURFACE_SIDE_STYLE('',(#5628));
#5624=SURFACE_SIDE_STYLE('',(#5629));
#5625=SURFACE_STYLE_FILL_AREA(#5630);
#5626=SURFACE_STYLE_FILL_AREA(#5631);
#5627=SURFACE_STYLE_FILL_AREA(#5632);
#5628=SURFACE_STYLE_FILL_AREA(#5633);
#5629=SURFACE_STYLE_FILL_AREA(#5634);
#5630=FILL_AREA_STYLE('Steel - Satin',(#5635));
#5631=FILL_AREA_STYLE('CAD Library Painted - Engineering blue',(#5636));
#5632=FILL_AREA_STYLE('CAD Library Painted - Steel gray',(#5637));
#5633=FILL_AREA_STYLE('CAD Library Painted - Graphite',(#5638));
#5634=FILL_AREA_STYLE('CAD Library Painted - Light blue',(#5639));
#5635=FILL_AREA_STYLE_COLOUR('Steel - Satin',#5640);
#5636=FILL_AREA_STYLE_COLOUR('CAD Library Painted - Engineering blue',#5641);
#5637=FILL_AREA_STYLE_COLOUR('CAD Library Painted - Steel gray',#5642);
#5638=FILL_AREA_STYLE_COLOUR('CAD Library Painted - Graphite',#5643);
#5639=FILL_AREA_STYLE_COLOUR('CAD Library Painted - Light blue',#5644);
#5640=COLOUR_RGB('Steel - Satin',0.627450980392157,0.627450980392157,0.627450980392157);
#5641=COLOUR_RGB('CAD Library Painted - Engineering blue',0.12156862745098,
0.356862745098039,0.6);
#5642=COLOUR_RGB('CAD Library Painted - Steel gray',0.592156862745098,0.631372549019608,
0.67843137254902);
#5643=COLOUR_RGB('CAD Library Painted - Graphite',0.168627450980392,0.192156862745098,
0.231372549019608);
#5644=COLOUR_RGB('CAD Library Painted - Light blue',0.286274509803922,0.552941176470588,
0.780392156862745);
#5645=COLOUR_RGB('Dark Blue',0.08,0.2,0.34);
#5646=FILL_AREA_STYLE_COLOUR('',#5645);
#5647=FILL_AREA_STYLE('',(#5646));
#5648=SURFACE_STYLE_FILL_AREA(#5647);
#5649=SURFACE_SIDE_STYLE('',(#5648));
#5650=SURFACE_STYLE_USAGE(.BOTH.,#5649);
#5651=PRESENTATION_STYLE_ASSIGNMENT((#5650));
#5652=COLOUR_RGB('Light Blue',0.38,0.62,0.78);
#5653=FILL_AREA_STYLE_COLOUR('',#5652);
#5654=FILL_AREA_STYLE('',(#5653));
#5655=SURFACE_STYLE_FILL_AREA(#5654);
#5656=SURFACE_SIDE_STYLE('',(#5655));
#5657=SURFACE_STYLE_USAGE(.BOTH.,#5656);
#5658=PRESENTATION_STYLE_ASSIGNMENT((#5657));
#5659=COLOUR_RGB('Sky Blue',0.24,0.69,0.87);
#5660=FILL_AREA_STYLE_COLOUR('',#5659);
#5661=FILL_AREA_STYLE('',(#5660));
#5662=SURFACE_STYLE_FILL_AREA(#5661);
#5663=SURFACE_SIDE_STYLE('',(#5662));
#5664=SURFACE_STYLE_USAGE(.BOTH.,#5663);
#5665=PRESENTATION_STYLE_ASSIGNMENT((#5664));
#5666=COLOUR_RGB('Grey',0.48,0.52,0.57);
#5667=FILL_AREA_STYLE_COLOUR('',#5666);
#5668=FILL_AREA_STYLE('',(#5667));
#5669=SURFACE_STYLE_FILL_AREA(#5668);
#5670=SURFACE_SIDE_STYLE('',(#5669));
#5671=SURFACE_STYLE_USAGE(.BOTH.,#5670);
#5672=PRESENTATION_STYLE_ASSIGNMENT((#5671));
#5673=COLOUR_RGB('Black',0.12,0.14,0.17);
#5674=FILL_AREA_STYLE_COLOUR('',#5673);
#5675=FILL_AREA_STYLE('',(#5674));
#5676=SURFACE_STYLE_FILL_AREA(#5675);
#5677=SURFACE_SIDE_STYLE('',(#5676));
#5678=SURFACE_STYLE_USAGE(.BOTH.,#5677);
#5679=PRESENTATION_STYLE_ASSIGNMENT((#5678));
#5680=COLOUR_RGB('Off White',0.89,0.88,0.83);
#5681=FILL_AREA_STYLE_COLOUR('',#5680);
#5682=FILL_AREA_STYLE('',(#5681));
#5683=SURFACE_STYLE_FILL_AREA(#5682);
#5684=SURFACE_SIDE_STYLE('',(#5683));
#5685=SURFACE_STYLE_USAGE(.BOTH.,#5684);
#5686=PRESENTATION_STYLE_ASSIGNMENT((#5685));
ENDSEC;
END-ISO-10303-21;
